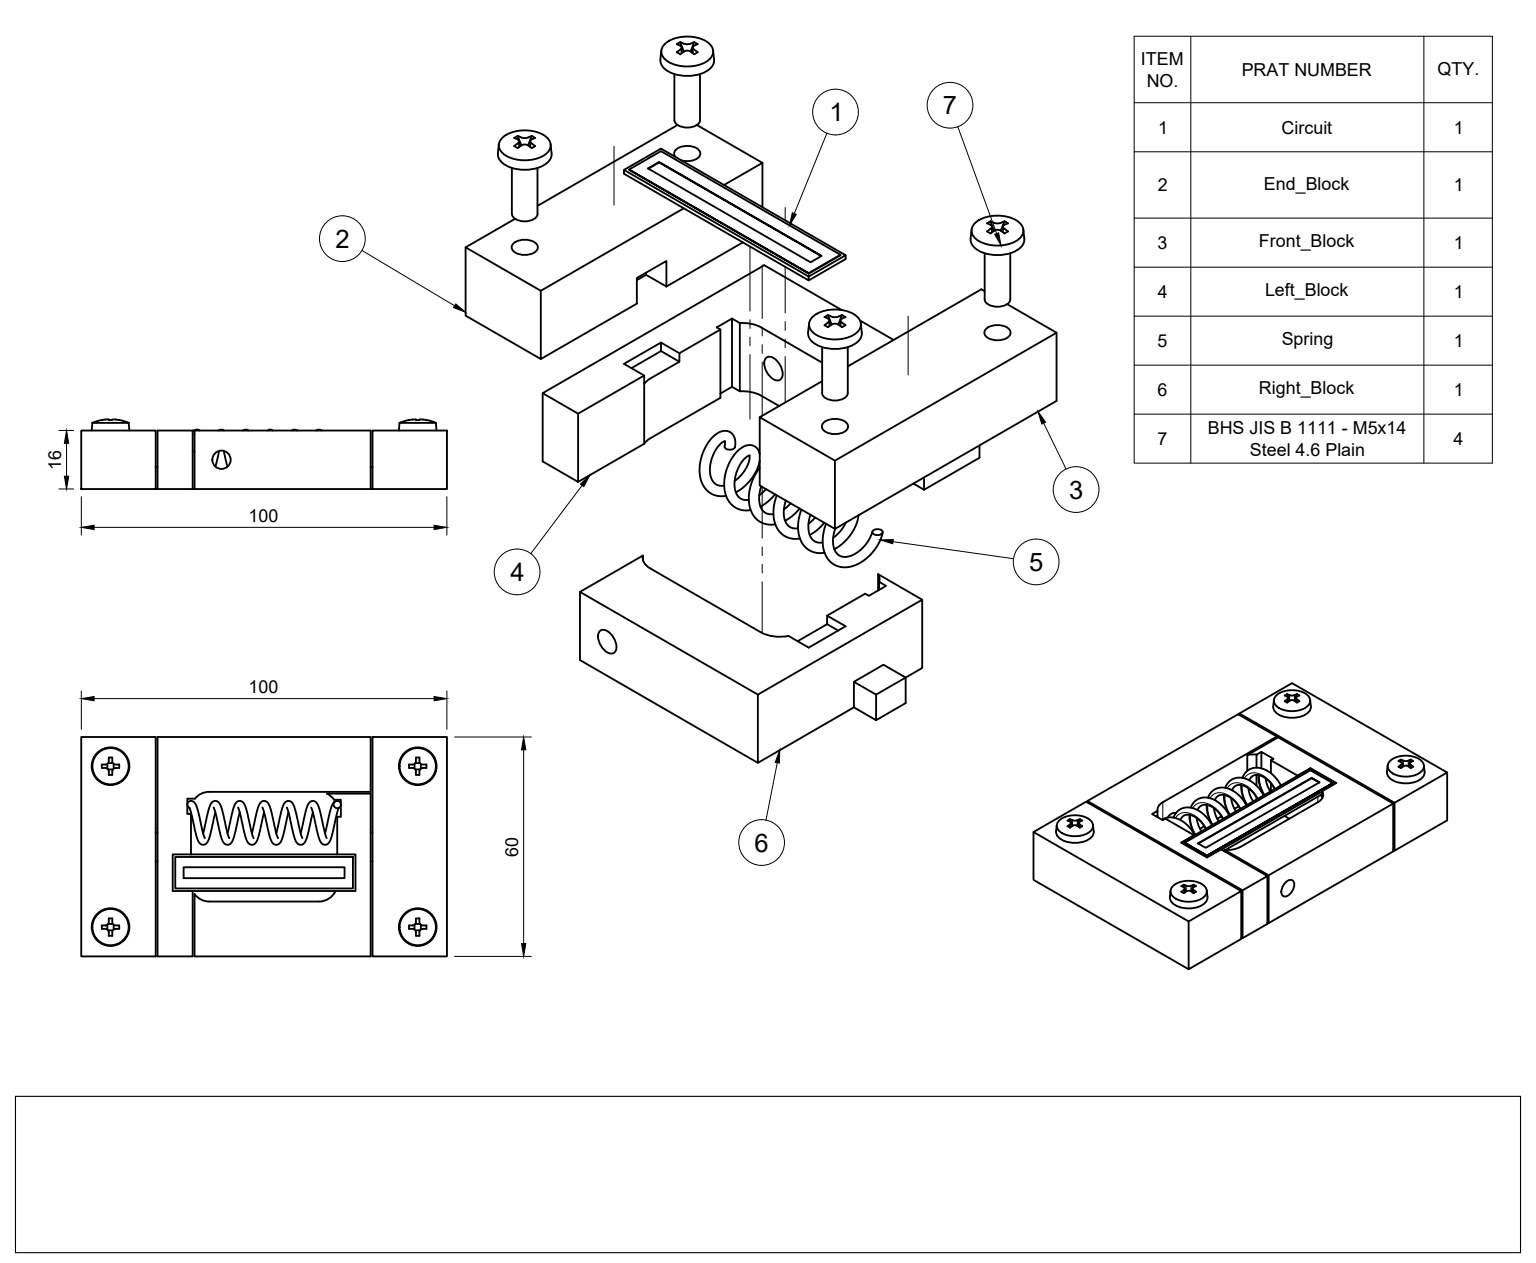
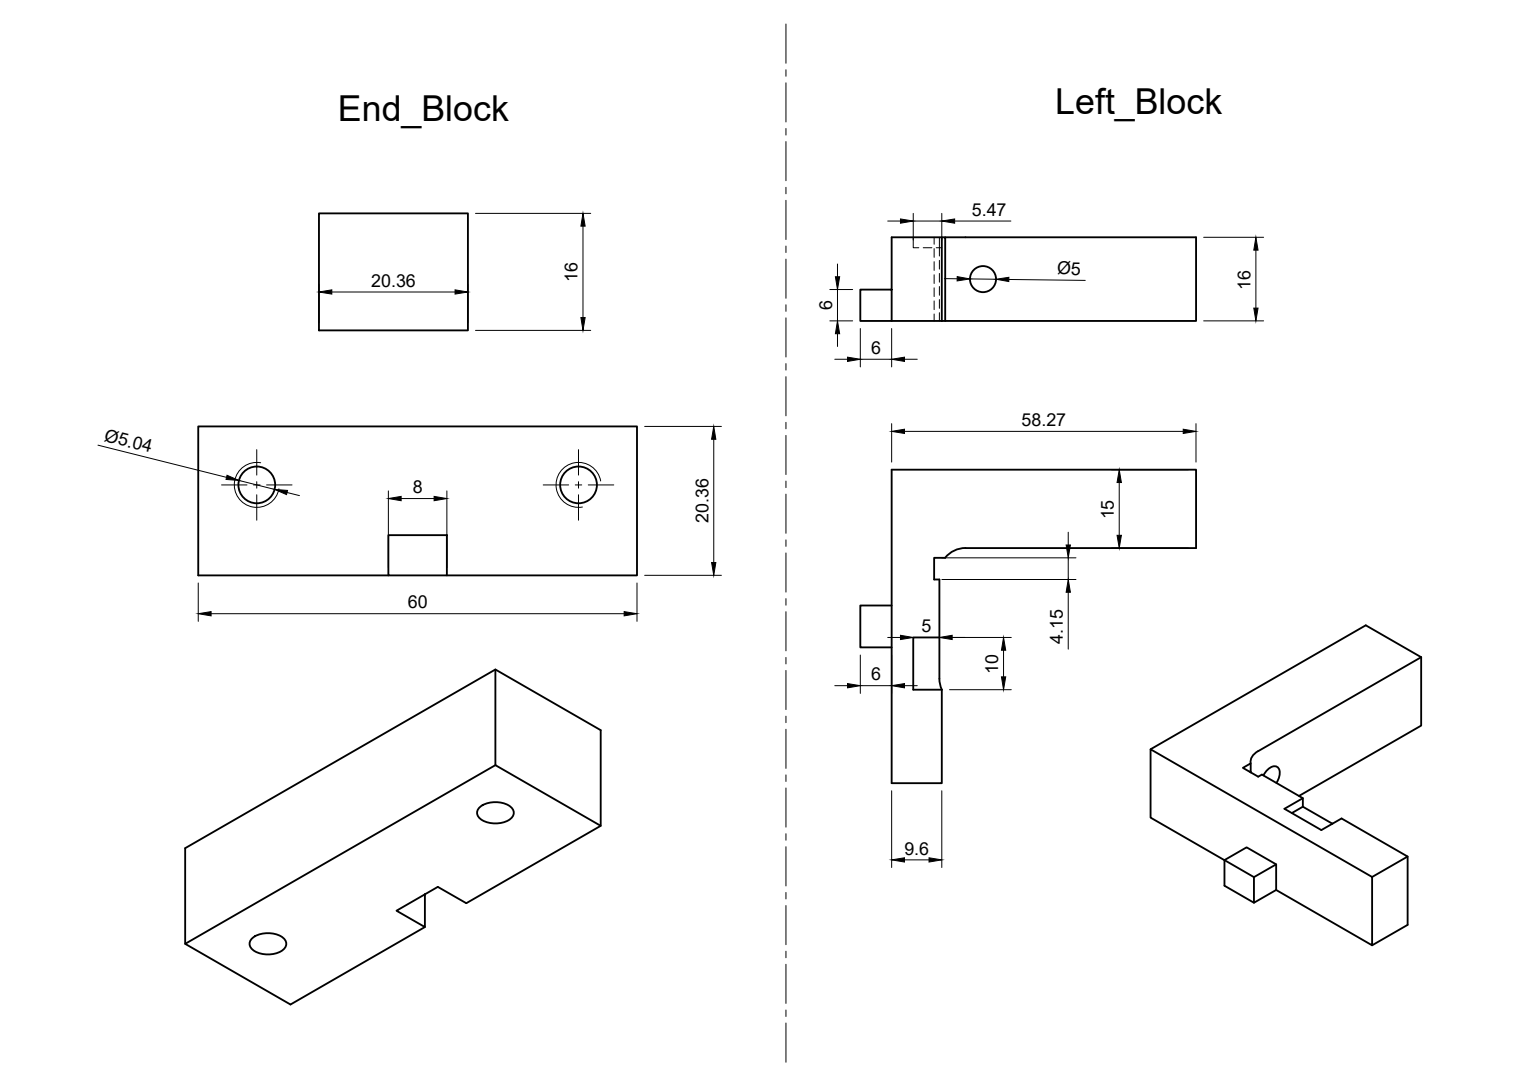
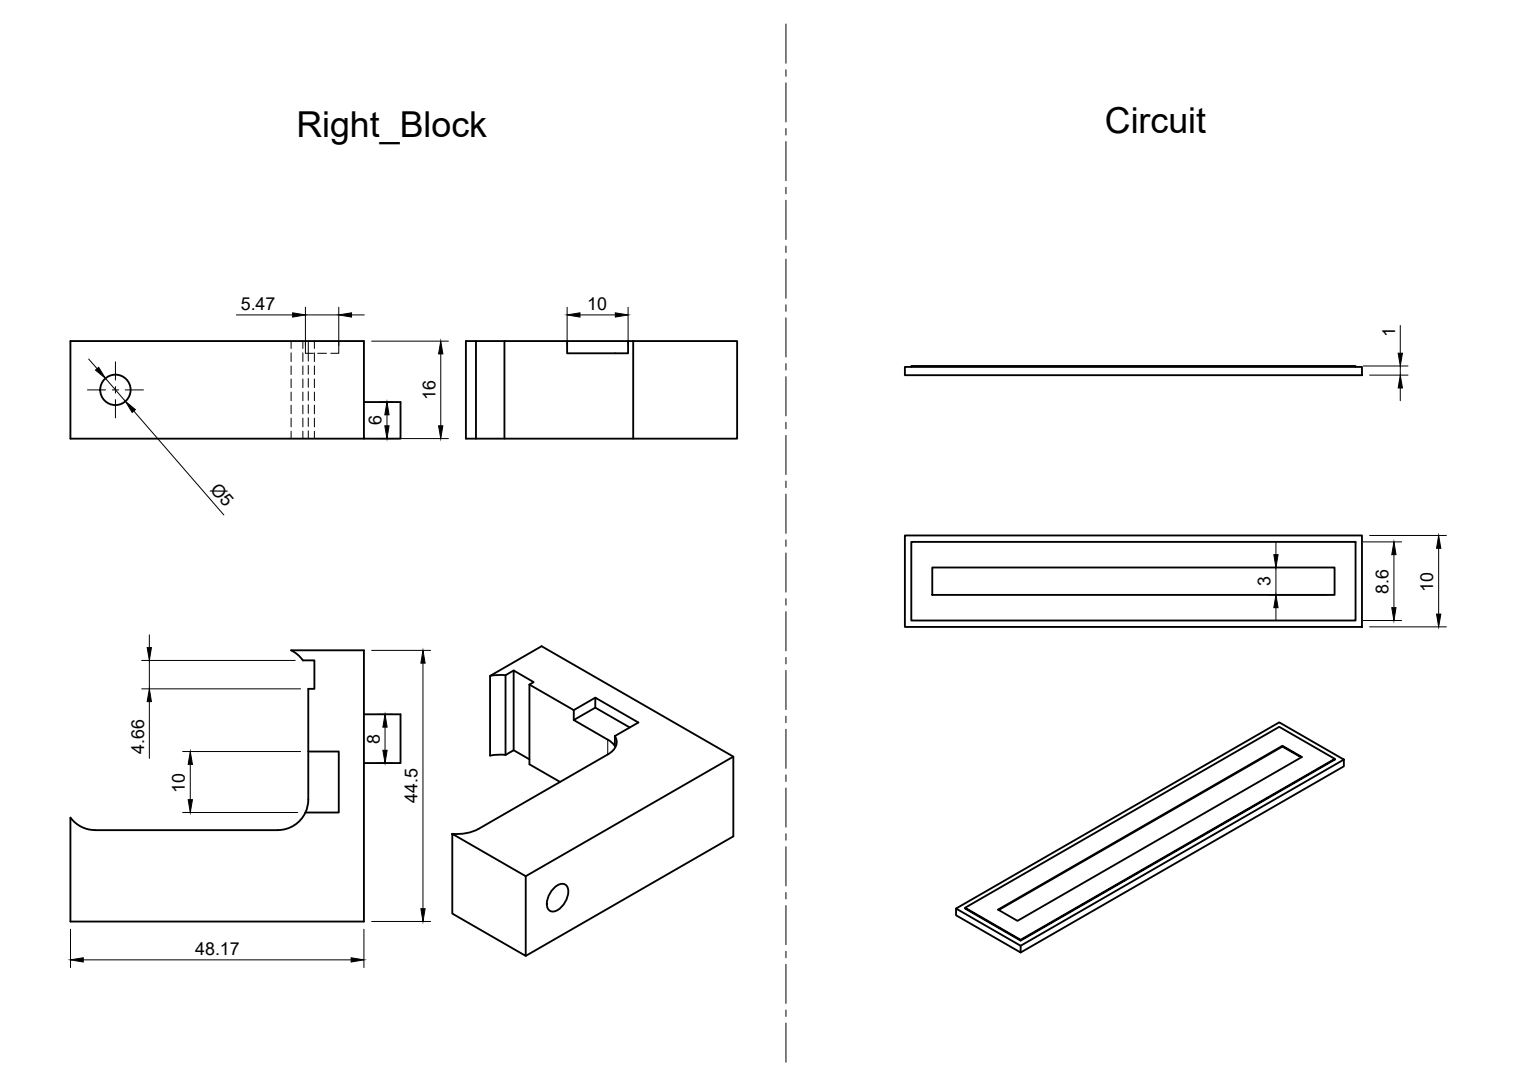
ISO-10303-21;
HEADER;
/* Generated by software containing ST-Developer
 * from STEP Tools, Inc. (www.steptools.com) 
 */

FILE_DESCRIPTION(
/* description */ (''),
/* implementation_level */ '2;1');

FILE_NAME(
/* name */ 'MAS-278',
/* time_stamp */ '2026-10-23T22:29:29+06:00',
/* author */ (''),
/* organization */ (''),
/* preprocessor_version */ 'ST-DEVELOPER v20.2',
/* originating_system */ 'Autodesk Translation Framework v15.15.0.0',
/* authorisation */ '');

FILE_SCHEMA (('AUTOMOTIVE_DESIGN { 1 0 10303 214 3 1 1 }'));
ENDSEC;

DATA;
#10=MECHANICAL_DESIGN_GEOMETRIC_PRESENTATION_REPRESENTATION('',(#72,#73,
#74,#75,#76,#77,#78,#79,#80,#81,#82,#83,#84),#7047);
#11=ITEM_DEFINED_TRANSFORMATION($,$,#3519,#3882);
#12=ITEM_DEFINED_TRANSFORMATION($,$,#3580,#3883);
#13=ITEM_DEFINED_TRANSFORMATION($,$,#3641,#3884);
#14=ITEM_DEFINED_TRANSFORMATION($,$,#3702,#3885);
#15=ITEM_DEFINED_TRANSFORMATION($,$,#3763,#3886);
#16=ITEM_DEFINED_TRANSFORMATION($,$,#3780,#3887);
#17=ITEM_DEFINED_TRANSFORMATION($,$,#3810,#3888);
#18=ITEM_DEFINED_TRANSFORMATION($,$,#3827,#3889);
#19=ITEM_DEFINED_TRANSFORMATION($,$,#3860,#3890);
#20=ITEM_DEFINED_TRANSFORMATION($,$,#3865,#3891);
#21=(
REPRESENTATION_RELATIONSHIP($,$,#7085,#7084)
REPRESENTATION_RELATIONSHIP_WITH_TRANSFORMATION(#11)
SHAPE_REPRESENTATION_RELATIONSHIP()
);
#22=(
REPRESENTATION_RELATIONSHIP($,$,#7086,#7084)
REPRESENTATION_RELATIONSHIP_WITH_TRANSFORMATION(#12)
SHAPE_REPRESENTATION_RELATIONSHIP()
);
#23=(
REPRESENTATION_RELATIONSHIP($,$,#7087,#7084)
REPRESENTATION_RELATIONSHIP_WITH_TRANSFORMATION(#13)
SHAPE_REPRESENTATION_RELATIONSHIP()
);
#24=(
REPRESENTATION_RELATIONSHIP($,$,#7088,#7084)
REPRESENTATION_RELATIONSHIP_WITH_TRANSFORMATION(#14)
SHAPE_REPRESENTATION_RELATIONSHIP()
);
#25=(
REPRESENTATION_RELATIONSHIP($,$,#7089,#7084)
REPRESENTATION_RELATIONSHIP_WITH_TRANSFORMATION(#15)
SHAPE_REPRESENTATION_RELATIONSHIP()
);
#26=(
REPRESENTATION_RELATIONSHIP($,$,#7090,#7084)
REPRESENTATION_RELATIONSHIP_WITH_TRANSFORMATION(#16)
SHAPE_REPRESENTATION_RELATIONSHIP()
);
#27=(
REPRESENTATION_RELATIONSHIP($,$,#7091,#7084)
REPRESENTATION_RELATIONSHIP_WITH_TRANSFORMATION(#17)
SHAPE_REPRESENTATION_RELATIONSHIP()
);
#28=(
REPRESENTATION_RELATIONSHIP($,$,#7092,#7084)
REPRESENTATION_RELATIONSHIP_WITH_TRANSFORMATION(#18)
SHAPE_REPRESENTATION_RELATIONSHIP()
);
#29=(
REPRESENTATION_RELATIONSHIP($,$,#7093,#7084)
REPRESENTATION_RELATIONSHIP_WITH_TRANSFORMATION(#19)
SHAPE_REPRESENTATION_RELATIONSHIP()
);
#30=(
REPRESENTATION_RELATIONSHIP($,$,#7094,#7084)
REPRESENTATION_RELATIONSHIP_WITH_TRANSFORMATION(#20)
SHAPE_REPRESENTATION_RELATIONSHIP()
);
#31=CONTEXT_DEPENDENT_SHAPE_REPRESENTATION(#21,#7074);
#32=CONTEXT_DEPENDENT_SHAPE_REPRESENTATION(#22,#7075);
#33=CONTEXT_DEPENDENT_SHAPE_REPRESENTATION(#23,#7076);
#34=CONTEXT_DEPENDENT_SHAPE_REPRESENTATION(#24,#7077);
#35=CONTEXT_DEPENDENT_SHAPE_REPRESENTATION(#25,#7078);
#36=CONTEXT_DEPENDENT_SHAPE_REPRESENTATION(#26,#7079);
#37=CONTEXT_DEPENDENT_SHAPE_REPRESENTATION(#27,#7080);
#38=CONTEXT_DEPENDENT_SHAPE_REPRESENTATION(#28,#7081);
#39=CONTEXT_DEPENDENT_SHAPE_REPRESENTATION(#29,#7082);
#40=CONTEXT_DEPENDENT_SHAPE_REPRESENTATION(#30,#7083);
#41=NEXT_ASSEMBLY_USAGE_OCCURRENCE('M5x14 Steel 4.6 Plain v1:1',
'M5x14 Steel 4.6 Plain v1:1','M5x14 Steel 4.6 Plain v1:1',#7096,#7097,
'M5x14 Steel 4.6 Plain v1:1');
#42=NEXT_ASSEMBLY_USAGE_OCCURRENCE('M5x14 Steel 4.6 Plain v1 (1):1',
'M5x14 Steel 4.6 Plain v1 (1):1','M5x14 Steel 4.6 Plain v1 (1):1',#7096,
#7098,'M5x14 Steel 4.6 Plain v1 (1):1');
#43=NEXT_ASSEMBLY_USAGE_OCCURRENCE('M5x14 Steel 4.6 Plain v1 (2):1',
'M5x14 Steel 4.6 Plain v1 (2):1','M5x14 Steel 4.6 Plain v1 (2):1',#7096,
#7099,'M5x14 Steel 4.6 Plain v1 (2):1');
#44=NEXT_ASSEMBLY_USAGE_OCCURRENCE('M5x14 Steel 4.6 Plain v1 (3):1',
'M5x14 Steel 4.6 Plain v1 (3):1','M5x14 Steel 4.6 Plain v1 (3):1',#7096,
#7100,'M5x14 Steel 4.6 Plain v1 (3):1');
#45=NEXT_ASSEMBLY_USAGE_OCCURRENCE('Front_Block:1','Front_Block:1',
'Front_Block:1',#7096,#7101,'Front_Block:1');
#46=NEXT_ASSEMBLY_USAGE_OCCURRENCE('Left_Block:1','Left_Block:1',
'Left_Block:1',#7096,#7102,'Left_Block:1');
#47=NEXT_ASSEMBLY_USAGE_OCCURRENCE('End_Block:1','End_Block:1',
'End_Block:1',#7096,#7103,'End_Block:1');
#48=NEXT_ASSEMBLY_USAGE_OCCURRENCE('Right_Block:1','Right_Block:1',
'Right_Block:1',#7096,#7104,'Right_Block:1');
#49=NEXT_ASSEMBLY_USAGE_OCCURRENCE('Spring:1','Spring:1','Spring:1',#7096,
#7105,'Spring:1');
#50=NEXT_ASSEMBLY_USAGE_OCCURRENCE('Circuit:1','Circuit:1','Circuit:1',
#7096,#7106,'Circuit:1');
#51=B_SPLINE_SURFACE_WITH_KNOTS('',3,3,((#6062,#6063,#6064,#6065,#6066,
#6067,#6068,#6069,#6070,#6071,#6072,#6073,#6074,#6075,#6076,#6077,#6078,
#6079,#6080,#6081,#6082,#6083,#6084,#6085,#6086,#6087,#6088,#6089,#6090,
#6091,#6092,#6093,#6094,#6095,#6096,#6097,#6098,#6099,#6100,#6101,#6102,
#6103,#6104,#6105,#6106,#6107,#6108,#6109,#6110,#6111,#6112,#6113,#6114,
#6115,#6116,#6117,#6118,#6119,#6120,#6121,#6122,#6123,#6124,#6125,#6126,
#6127,#6128,#6129,#6130,#6131,#6132,#6133,#6134,#6135,#6136,#6137,#6138,
#6139,#6140),(#6141,#6142,#6143,#6144,#6145,#6146,#6147,#6148,#6149,#6150,
#6151,#6152,#6153,#6154,#6155,#6156,#6157,#6158,#6159,#6160,#6161,#6162,
#6163,#6164,#6165,#6166,#6167,#6168,#6169,#6170,#6171,#6172,#6173,#6174,
#6175,#6176,#6177,#6178,#6179,#6180,#6181,#6182,#6183,#6184,#6185,#6186,
#6187,#6188,#6189,#6190,#6191,#6192,#6193,#6194,#6195,#6196,#6197,#6198,
#6199,#6200,#6201,#6202,#6203,#6204,#6205,#6206,#6207,#6208,#6209,#6210,
#6211,#6212,#6213,#6214,#6215,#6216,#6217,#6218,#6219),(#6220,#6221,#6222,
#6223,#6224,#6225,#6226,#6227,#6228,#6229,#6230,#6231,#6232,#6233,#6234,
#6235,#6236,#6237,#6238,#6239,#6240,#6241,#6242,#6243,#6244,#6245,#6246,
#6247,#6248,#6249,#6250,#6251,#6252,#6253,#6254,#6255,#6256,#6257,#6258,
#6259,#6260,#6261,#6262,#6263,#6264,#6265,#6266,#6267,#6268,#6269,#6270,
#6271,#6272,#6273,#6274,#6275,#6276,#6277,#6278,#6279,#6280,#6281,#6282,
#6283,#6284,#6285,#6286,#6287,#6288,#6289,#6290,#6291,#6292,#6293,#6294,
#6295,#6296,#6297,#6298),(#6299,#6300,#6301,#6302,#6303,#6304,#6305,#6306,
#6307,#6308,#6309,#6310,#6311,#6312,#6313,#6314,#6315,#6316,#6317,#6318,
#6319,#6320,#6321,#6322,#6323,#6324,#6325,#6326,#6327,#6328,#6329,#6330,
#6331,#6332,#6333,#6334,#6335,#6336,#6337,#6338,#6339,#6340,#6341,#6342,
#6343,#6344,#6345,#6346,#6347,#6348,#6349,#6350,#6351,#6352,#6353,#6354,
#6355,#6356,#6357,#6358,#6359,#6360,#6361,#6362,#6363,#6364,#6365,#6366,
#6367,#6368,#6369,#6370,#6371,#6372,#6373,#6374,#6375,#6376,#6377),(#6378,
#6379,#6380,#6381,#6382,#6383,#6384,#6385,#6386,#6387,#6388,#6389,#6390,
#6391,#6392,#6393,#6394,#6395,#6396,#6397,#6398,#6399,#6400,#6401,#6402,
#6403,#6404,#6405,#6406,#6407,#6408,#6409,#6410,#6411,#6412,#6413,#6414,
#6415,#6416,#6417,#6418,#6419,#6420,#6421,#6422,#6423,#6424,#6425,#6426,
#6427,#6428,#6429,#6430,#6431,#6432,#6433,#6434,#6435,#6436,#6437,#6438,
#6439,#6440,#6441,#6442,#6443,#6444,#6445,#6446,#6447,#6448,#6449,#6450,
#6451,#6452,#6453,#6454,#6455,#6456),(#6457,#6458,#6459,#6460,#6461,#6462,
#6463,#6464,#6465,#6466,#6467,#6468,#6469,#6470,#6471,#6472,#6473,#6474,
#6475,#6476,#6477,#6478,#6479,#6480,#6481,#6482,#6483,#6484,#6485,#6486,
#6487,#6488,#6489,#6490,#6491,#6492,#6493,#6494,#6495,#6496,#6497,#6498,
#6499,#6500,#6501,#6502,#6503,#6504,#6505,#6506,#6507,#6508,#6509,#6510,
#6511,#6512,#6513,#6514,#6515,#6516,#6517,#6518,#6519,#6520,#6521,#6522,
#6523,#6524,#6525,#6526,#6527,#6528,#6529,#6530,#6531,#6532,#6533,#6534,
#6535),(#6536,#6537,#6538,#6539,#6540,#6541,#6542,#6543,#6544,#6545,#6546,
#6547,#6548,#6549,#6550,#6551,#6552,#6553,#6554,#6555,#6556,#6557,#6558,
#6559,#6560,#6561,#6562,#6563,#6564,#6565,#6566,#6567,#6568,#6569,#6570,
#6571,#6572,#6573,#6574,#6575,#6576,#6577,#6578,#6579,#6580,#6581,#6582,
#6583,#6584,#6585,#6586,#6587,#6588,#6589,#6590,#6591,#6592,#6593,#6594,
#6595,#6596,#6597,#6598,#6599,#6600,#6601,#6602,#6603,#6604,#6605,#6606,
#6607,#6608,#6609,#6610,#6611,#6612,#6613,#6614),(#6615,#6616,#6617,#6618,
#6619,#6620,#6621,#6622,#6623,#6624,#6625,#6626,#6627,#6628,#6629,#6630,
#6631,#6632,#6633,#6634,#6635,#6636,#6637,#6638,#6639,#6640,#6641,#6642,
#6643,#6644,#6645,#6646,#6647,#6648,#6649,#6650,#6651,#6652,#6653,#6654,
#6655,#6656,#6657,#6658,#6659,#6660,#6661,#6662,#6663,#6664,#6665,#6666,
#6667,#6668,#6669,#6670,#6671,#6672,#6673,#6674,#6675,#6676,#6677,#6678,
#6679,#6680,#6681,#6682,#6683,#6684,#6685,#6686,#6687,#6688,#6689,#6690,
#6691,#6692,#6693),(#6694,#6695,#6696,#6697,#6698,#6699,#6700,#6701,#6702,
#6703,#6704,#6705,#6706,#6707,#6708,#6709,#6710,#6711,#6712,#6713,#6714,
#6715,#6716,#6717,#6718,#6719,#6720,#6721,#6722,#6723,#6724,#6725,#6726,
#6727,#6728,#6729,#6730,#6731,#6732,#6733,#6734,#6735,#6736,#6737,#6738,
#6739,#6740,#6741,#6742,#6743,#6744,#6745,#6746,#6747,#6748,#6749,#6750,
#6751,#6752,#6753,#6754,#6755,#6756,#6757,#6758,#6759,#6760,#6761,#6762,
#6763,#6764,#6765,#6766,#6767,#6768,#6769,#6770,#6771,#6772),(#6773,#6774,
#6775,#6776,#6777,#6778,#6779,#6780,#6781,#6782,#6783,#6784,#6785,#6786,
#6787,#6788,#6789,#6790,#6791,#6792,#6793,#6794,#6795,#6796,#6797,#6798,
#6799,#6800,#6801,#6802,#6803,#6804,#6805,#6806,#6807,#6808,#6809,#6810,
#6811,#6812,#6813,#6814,#6815,#6816,#6817,#6818,#6819,#6820,#6821,#6822,
#6823,#6824,#6825,#6826,#6827,#6828,#6829,#6830,#6831,#6832,#6833,#6834,
#6835,#6836,#6837,#6838,#6839,#6840,#6841,#6842,#6843,#6844,#6845,#6846,
#6847,#6848,#6849,#6850,#6851)),.UNSPECIFIED.,.T.,.F.,.F.,(4,1,1,1,1,1,
1,4),(4,1,1,1,1,1,1,1,1,1,1,1,1,1,1,1,1,1,1,1,1,1,1,1,1,1,1,1,1,1,1,1,1,
1,1,1,1,1,1,1,1,1,1,1,1,1,1,1,1,1,1,1,1,1,1,1,1,1,1,1,1,1,1,1,1,1,1,1,1,
1,1,1,1,1,1,1,4),(-3.14159265358979,-2.24399475256414,-1.34639685153848,
-0.448798950512828,0.448798950512828,1.34639685153848,2.24399475256414,
3.14159265358979),(0.,0.496040945303652,0.992081890607303,1.48812283591095,
1.98416378121461,2.48020472651826,2.97624567182191,3.47228661712556,3.96832756242921,
4.46436850773286,4.96040945303652,5.45645039834017,5.95249134364382,6.44853228894747,
6.94457323425112,7.44061417955477,7.93665512485842,8.43269607016208,8.92873701546573,
9.42477796076938,9.92081890607303,10.4168598513767,10.9129007966803,11.408941741984,
11.9049826872876,12.4010236325913,12.8970645778949,13.3931055231986,13.8891464685022,
14.3851874138059,14.8812283591095,15.3772693044132,15.8733102497168,16.3693511950205,
16.8653921403242,17.3614330856278,17.8574740309315,18.3535149762351,18.8495559215388,
19.3455968668424,19.8416378121461,20.3376787574497,20.8337197027534,21.329760648057,
21.8258015933607,22.3218425386643,22.817883483968,23.3139244292716,23.8099653745753,
24.3060063198789,24.8020472651826,25.2980882104862,25.7941291557899,26.2901701010935,
26.7862110463972,27.2822519917008,27.7782929370045,28.2743338823081,28.7703748276118,
29.2664157729154,29.7624567182191,30.2584976635227,30.7545386088264,31.25057955413,
31.7466204994337,32.2426614447374,32.738702390041,33.2347433353447,33.7307842806483,
34.226825225952,34.7228661712556,35.2189071165593,35.7149480618629,36.2109890071666,
36.7070299524702,37.2030708977739,37.6991118430775),.UNSPECIFIED.);
#52=SHAPE_REPRESENTATION_RELATIONSHIP('SRR','None',#7085,#62);
#53=SHAPE_REPRESENTATION_RELATIONSHIP('SRR','None',#7086,#63);
#54=SHAPE_REPRESENTATION_RELATIONSHIP('SRR','None',#7087,#64);
#55=SHAPE_REPRESENTATION_RELATIONSHIP('SRR','None',#7088,#65);
#56=SHAPE_REPRESENTATION_RELATIONSHIP('SRR','None',#7089,#66);
#57=SHAPE_REPRESENTATION_RELATIONSHIP('SRR','None',#7090,#67);
#58=SHAPE_REPRESENTATION_RELATIONSHIP('SRR','None',#7091,#68);
#59=SHAPE_REPRESENTATION_RELATIONSHIP('SRR','None',#7092,#69);
#60=SHAPE_REPRESENTATION_RELATIONSHIP('SRR','None',#7093,#70);
#61=SHAPE_REPRESENTATION_RELATIONSHIP('SRR','None',#7094,#71);
#62=ADVANCED_BREP_SHAPE_REPRESENTATION('',(#85),#7037);
#63=ADVANCED_BREP_SHAPE_REPRESENTATION('',(#86),#7038);
#64=ADVANCED_BREP_SHAPE_REPRESENTATION('',(#87),#7039);
#65=ADVANCED_BREP_SHAPE_REPRESENTATION('',(#88),#7040);
#66=ADVANCED_BREP_SHAPE_REPRESENTATION('',(#89),#7041);
#67=ADVANCED_BREP_SHAPE_REPRESENTATION('',(#90),#7042);
#68=ADVANCED_BREP_SHAPE_REPRESENTATION('',(#91),#7043);
#69=ADVANCED_BREP_SHAPE_REPRESENTATION('',(#92),#7044);
#70=ADVANCED_BREP_SHAPE_REPRESENTATION('',(#93),#7045);
#71=ADVANCED_BREP_SHAPE_REPRESENTATION('',(#94),#7046);
#72=STYLED_ITEM('',(#7212),#85);
#73=STYLED_ITEM('',(#7212),#86);
#74=STYLED_ITEM('',(#7212),#87);
#75=STYLED_ITEM('',(#7212),#88);
#76=STYLED_ITEM('',(#7177),#89);
#77=STYLED_ITEM('',(#7177),#90);
#78=STYLED_ITEM('',(#7177),#91);
#79=STYLED_ITEM('',(#7177),#92);
#80=STYLED_ITEM('',(#7198),#93);
#81=STYLED_ITEM('',(#7212),#3385);
#82=STYLED_ITEM('',(#7212),#3392);
#83=STYLED_ITEM('',(#7212),#3395);
#84=STYLED_ITEM('',(#7212),#94);
#85=MANIFOLD_SOLID_BREP('Body1',#3397);
#86=MANIFOLD_SOLID_BREP('Body1',#3398);
#87=MANIFOLD_SOLID_BREP('Body1',#3399);
#88=MANIFOLD_SOLID_BREP('Body1',#3400);
#89=MANIFOLD_SOLID_BREP('Front_Block',#3401);
#90=MANIFOLD_SOLID_BREP('Left_Block',#3402);
#91=MANIFOLD_SOLID_BREP('End_Block',#3403);
#92=MANIFOLD_SOLID_BREP('Right_Block',#3404);
#93=MANIFOLD_SOLID_BREP('Spring',#3405);
#94=MANIFOLD_SOLID_BREP('Circuit',#3406);
#95=SPHERICAL_SURFACE('',#3575,12.8319377609308);
#96=SPHERICAL_SURFACE('',#3636,12.8319377609308);
#97=SPHERICAL_SURFACE('',#3697,12.8319377609308);
#98=SPHERICAL_SURFACE('',#3758,12.8319377609308);
#99=CONICAL_SURFACE('',#3570,2.33923048454133,0.261799387799147);
#100=CONICAL_SURFACE('',#3579,5.05813690328693,0.0872664626099692);
#101=CONICAL_SURFACE('',#3631,2.33923048454133,0.261799387799147);
#102=CONICAL_SURFACE('',#3640,5.05813690328693,0.0872664626099692);
#103=CONICAL_SURFACE('',#3692,2.33923048454133,0.261799387799147);
#104=CONICAL_SURFACE('',#3701,5.05813690328693,0.0872664626099692);
#105=CONICAL_SURFACE('',#3753,2.33923048454133,0.261799387799147);
#106=CONICAL_SURFACE('',#3762,5.05813690328693,0.0872664626099692);
#107=FACE_BOUND('',#474,.T.);
#108=FACE_BOUND('',#500,.T.);
#109=FACE_BOUND('',#526,.T.);
#110=FACE_BOUND('',#552,.T.);
#111=FACE_BOUND('',#564,.T.);
#112=FACE_BOUND('',#565,.T.);
#113=FACE_BOUND('',#568,.T.);
#114=FACE_BOUND('',#569,.T.);
#115=FACE_BOUND('',#590,.T.);
#116=FACE_BOUND('',#593,.T.);
#117=FACE_BOUND('',#606,.T.);
#118=FACE_BOUND('',#607,.T.);
#119=FACE_BOUND('',#610,.T.);
#120=FACE_BOUND('',#611,.T.);
#121=FACE_BOUND('',#626,.T.);
#122=FACE_BOUND('',#639,.T.);
#123=FACE_BOUND('',#649,.T.);
#124=FACE_BOUND('',#660,.T.);
#125=TOROIDAL_SURFACE('',#3562,2.37846096908266,0.2);
#126=TOROIDAL_SURFACE('',#3623,2.37846096908266,0.2);
#127=TOROIDAL_SURFACE('',#3684,2.37846096908266,0.2);
#128=TOROIDAL_SURFACE('',#3745,2.37846096908266,0.2);
#129=PLANE('',#3524);
#130=PLANE('',#3526);
#131=PLANE('',#3529);
#132=PLANE('',#3534);
#133=PLANE('',#3536);
#134=PLANE('',#3539);
#135=PLANE('',#3545);
#136=PLANE('',#3550);
#137=PLANE('',#3552);
#138=PLANE('',#3554);
#139=PLANE('',#3557);
#140=PLANE('',#3559);
#141=PLANE('',#3561);
#142=PLANE('',#3566);
#143=PLANE('',#3574);
#144=PLANE('',#3585);
#145=PLANE('',#3587);
#146=PLANE('',#3590);
#147=PLANE('',#3595);
#148=PLANE('',#3597);
#149=PLANE('',#3600);
#150=PLANE('',#3606);
#151=PLANE('',#3611);
#152=PLANE('',#3613);
#153=PLANE('',#3615);
#154=PLANE('',#3618);
#155=PLANE('',#3620);
#156=PLANE('',#3622);
#157=PLANE('',#3627);
#158=PLANE('',#3635);
#159=PLANE('',#3646);
#160=PLANE('',#3648);
#161=PLANE('',#3651);
#162=PLANE('',#3656);
#163=PLANE('',#3658);
#164=PLANE('',#3661);
#165=PLANE('',#3667);
#166=PLANE('',#3672);
#167=PLANE('',#3674);
#168=PLANE('',#3676);
#169=PLANE('',#3679);
#170=PLANE('',#3681);
#171=PLANE('',#3683);
#172=PLANE('',#3688);
#173=PLANE('',#3696);
#174=PLANE('',#3707);
#175=PLANE('',#3709);
#176=PLANE('',#3712);
#177=PLANE('',#3717);
#178=PLANE('',#3719);
#179=PLANE('',#3722);
#180=PLANE('',#3728);
#181=PLANE('',#3733);
#182=PLANE('',#3735);
#183=PLANE('',#3737);
#184=PLANE('',#3740);
#185=PLANE('',#3742);
#186=PLANE('',#3744);
#187=PLANE('',#3749);
#188=PLANE('',#3757);
#189=PLANE('',#3764);
#190=PLANE('',#3765);
#191=PLANE('',#3766);
#192=PLANE('',#3767);
#193=PLANE('',#3768);
#194=PLANE('',#3771);
#195=PLANE('',#3772);
#196=PLANE('',#3775);
#197=PLANE('',#3776);
#198=PLANE('',#3779);
#199=PLANE('',#3781);
#200=PLANE('',#3782);
#201=PLANE('',#3783);
#202=PLANE('',#3784);
#203=PLANE('',#3785);
#204=PLANE('',#3789);
#205=PLANE('',#3790);
#206=PLANE('',#3791);
#207=PLANE('',#3792);
#208=PLANE('',#3793);
#209=PLANE('',#3794);
#210=PLANE('',#3795);
#211=PLANE('',#3796);
#212=PLANE('',#3798);
#213=PLANE('',#3802);
#214=PLANE('',#3803);
#215=PLANE('',#3805);
#216=PLANE('',#3806);
#217=PLANE('',#3808);
#218=PLANE('',#3809);
#219=PLANE('',#3811);
#220=PLANE('',#3812);
#221=PLANE('',#3813);
#222=PLANE('',#3814);
#223=PLANE('',#3815);
#224=PLANE('',#3816);
#225=PLANE('',#3819);
#226=PLANE('',#3820);
#227=PLANE('',#3823);
#228=PLANE('',#3826);
#229=PLANE('',#3828);
#230=PLANE('',#3829);
#231=PLANE('',#3830);
#232=PLANE('',#3831);
#233=PLANE('',#3832);
#234=PLANE('',#3833);
#235=PLANE('',#3834);
#236=PLANE('',#3838);
#237=PLANE('',#3841);
#238=PLANE('',#3843);
#239=PLANE('',#3847);
#240=PLANE('',#3848);
#241=PLANE('',#3849);
#242=PLANE('',#3850);
#243=PLANE('',#3853);
#244=PLANE('',#3854);
#245=PLANE('',#3855);
#246=PLANE('',#3858);
#247=PLANE('',#3859);
#248=PLANE('',#3863);
#249=PLANE('',#3864);
#250=PLANE('',#3866);
#251=PLANE('',#3867);
#252=PLANE('',#3868);
#253=PLANE('',#3869);
#254=PLANE('',#3870);
#255=PLANE('',#3871);
#256=PLANE('',#3872);
#257=PLANE('',#3873);
#258=PLANE('',#3874);
#259=PLANE('',#3875);
#260=PLANE('',#3876);
#261=PLANE('',#3877);
#262=PLANE('',#3878);
#263=PLANE('',#3879);
#264=PLANE('',#3880);
#265=PLANE('',#3881);
#266=FACE_OUTER_BOUND('',#455,.T.);
#267=FACE_OUTER_BOUND('',#456,.T.);
#268=FACE_OUTER_BOUND('',#457,.T.);
#269=FACE_OUTER_BOUND('',#458,.T.);
#270=FACE_OUTER_BOUND('',#459,.T.);
#271=FACE_OUTER_BOUND('',#460,.T.);
#272=FACE_OUTER_BOUND('',#461,.T.);
#273=FACE_OUTER_BOUND('',#462,.T.);
#274=FACE_OUTER_BOUND('',#463,.T.);
#275=FACE_OUTER_BOUND('',#464,.T.);
#276=FACE_OUTER_BOUND('',#465,.T.);
#277=FACE_OUTER_BOUND('',#466,.T.);
#278=FACE_OUTER_BOUND('',#467,.T.);
#279=FACE_OUTER_BOUND('',#468,.T.);
#280=FACE_OUTER_BOUND('',#469,.T.);
#281=FACE_OUTER_BOUND('',#470,.T.);
#282=FACE_OUTER_BOUND('',#471,.T.);
#283=FACE_OUTER_BOUND('',#472,.T.);
#284=FACE_OUTER_BOUND('',#473,.T.);
#285=FACE_OUTER_BOUND('',#475,.T.);
#286=FACE_OUTER_BOUND('',#476,.T.);
#287=FACE_OUTER_BOUND('',#477,.T.);
#288=FACE_OUTER_BOUND('',#478,.T.);
#289=FACE_OUTER_BOUND('',#479,.T.);
#290=FACE_OUTER_BOUND('',#480,.T.);
#291=FACE_OUTER_BOUND('',#481,.T.);
#292=FACE_OUTER_BOUND('',#482,.T.);
#293=FACE_OUTER_BOUND('',#483,.T.);
#294=FACE_OUTER_BOUND('',#484,.T.);
#295=FACE_OUTER_BOUND('',#485,.T.);
#296=FACE_OUTER_BOUND('',#486,.T.);
#297=FACE_OUTER_BOUND('',#487,.T.);
#298=FACE_OUTER_BOUND('',#488,.T.);
#299=FACE_OUTER_BOUND('',#489,.T.);
#300=FACE_OUTER_BOUND('',#490,.T.);
#301=FACE_OUTER_BOUND('',#491,.T.);
#302=FACE_OUTER_BOUND('',#492,.T.);
#303=FACE_OUTER_BOUND('',#493,.T.);
#304=FACE_OUTER_BOUND('',#494,.T.);
#305=FACE_OUTER_BOUND('',#495,.T.);
#306=FACE_OUTER_BOUND('',#496,.T.);
#307=FACE_OUTER_BOUND('',#497,.T.);
#308=FACE_OUTER_BOUND('',#498,.T.);
#309=FACE_OUTER_BOUND('',#499,.T.);
#310=FACE_OUTER_BOUND('',#501,.T.);
#311=FACE_OUTER_BOUND('',#502,.T.);
#312=FACE_OUTER_BOUND('',#503,.T.);
#313=FACE_OUTER_BOUND('',#504,.T.);
#314=FACE_OUTER_BOUND('',#505,.T.);
#315=FACE_OUTER_BOUND('',#506,.T.);
#316=FACE_OUTER_BOUND('',#507,.T.);
#317=FACE_OUTER_BOUND('',#508,.T.);
#318=FACE_OUTER_BOUND('',#509,.T.);
#319=FACE_OUTER_BOUND('',#510,.T.);
#320=FACE_OUTER_BOUND('',#511,.T.);
#321=FACE_OUTER_BOUND('',#512,.T.);
#322=FACE_OUTER_BOUND('',#513,.T.);
#323=FACE_OUTER_BOUND('',#514,.T.);
#324=FACE_OUTER_BOUND('',#515,.T.);
#325=FACE_OUTER_BOUND('',#516,.T.);
#326=FACE_OUTER_BOUND('',#517,.T.);
#327=FACE_OUTER_BOUND('',#518,.T.);
#328=FACE_OUTER_BOUND('',#519,.T.);
#329=FACE_OUTER_BOUND('',#520,.T.);
#330=FACE_OUTER_BOUND('',#521,.T.);
#331=FACE_OUTER_BOUND('',#522,.T.);
#332=FACE_OUTER_BOUND('',#523,.T.);
#333=FACE_OUTER_BOUND('',#524,.T.);
#334=FACE_OUTER_BOUND('',#525,.T.);
#335=FACE_OUTER_BOUND('',#527,.T.);
#336=FACE_OUTER_BOUND('',#528,.T.);
#337=FACE_OUTER_BOUND('',#529,.T.);
#338=FACE_OUTER_BOUND('',#530,.T.);
#339=FACE_OUTER_BOUND('',#531,.T.);
#340=FACE_OUTER_BOUND('',#532,.T.);
#341=FACE_OUTER_BOUND('',#533,.T.);
#342=FACE_OUTER_BOUND('',#534,.T.);
#343=FACE_OUTER_BOUND('',#535,.T.);
#344=FACE_OUTER_BOUND('',#536,.T.);
#345=FACE_OUTER_BOUND('',#537,.T.);
#346=FACE_OUTER_BOUND('',#538,.T.);
#347=FACE_OUTER_BOUND('',#539,.T.);
#348=FACE_OUTER_BOUND('',#540,.T.);
#349=FACE_OUTER_BOUND('',#541,.T.);
#350=FACE_OUTER_BOUND('',#542,.T.);
#351=FACE_OUTER_BOUND('',#543,.T.);
#352=FACE_OUTER_BOUND('',#544,.T.);
#353=FACE_OUTER_BOUND('',#545,.T.);
#354=FACE_OUTER_BOUND('',#546,.T.);
#355=FACE_OUTER_BOUND('',#547,.T.);
#356=FACE_OUTER_BOUND('',#548,.T.);
#357=FACE_OUTER_BOUND('',#549,.T.);
#358=FACE_OUTER_BOUND('',#550,.T.);
#359=FACE_OUTER_BOUND('',#551,.T.);
#360=FACE_OUTER_BOUND('',#553,.T.);
#361=FACE_OUTER_BOUND('',#554,.T.);
#362=FACE_OUTER_BOUND('',#555,.T.);
#363=FACE_OUTER_BOUND('',#556,.T.);
#364=FACE_OUTER_BOUND('',#557,.T.);
#365=FACE_OUTER_BOUND('',#558,.T.);
#366=FACE_OUTER_BOUND('',#559,.T.);
#367=FACE_OUTER_BOUND('',#560,.T.);
#368=FACE_OUTER_BOUND('',#561,.T.);
#369=FACE_OUTER_BOUND('',#562,.T.);
#370=FACE_OUTER_BOUND('',#563,.T.);
#371=FACE_OUTER_BOUND('',#566,.T.);
#372=FACE_OUTER_BOUND('',#567,.T.);
#373=FACE_OUTER_BOUND('',#570,.T.);
#374=FACE_OUTER_BOUND('',#571,.T.);
#375=FACE_OUTER_BOUND('',#572,.T.);
#376=FACE_OUTER_BOUND('',#573,.T.);
#377=FACE_OUTER_BOUND('',#574,.T.);
#378=FACE_OUTER_BOUND('',#575,.T.);
#379=FACE_OUTER_BOUND('',#576,.T.);
#380=FACE_OUTER_BOUND('',#577,.T.);
#381=FACE_OUTER_BOUND('',#578,.T.);
#382=FACE_OUTER_BOUND('',#579,.T.);
#383=FACE_OUTER_BOUND('',#580,.T.);
#384=FACE_OUTER_BOUND('',#581,.T.);
#385=FACE_OUTER_BOUND('',#582,.T.);
#386=FACE_OUTER_BOUND('',#583,.T.);
#387=FACE_OUTER_BOUND('',#584,.T.);
#388=FACE_OUTER_BOUND('',#585,.T.);
#389=FACE_OUTER_BOUND('',#586,.T.);
#390=FACE_OUTER_BOUND('',#587,.T.);
#391=FACE_OUTER_BOUND('',#588,.T.);
#392=FACE_OUTER_BOUND('',#589,.T.);
#393=FACE_OUTER_BOUND('',#591,.T.);
#394=FACE_OUTER_BOUND('',#592,.T.);
#395=FACE_OUTER_BOUND('',#594,.T.);
#396=FACE_OUTER_BOUND('',#595,.T.);
#397=FACE_OUTER_BOUND('',#596,.T.);
#398=FACE_OUTER_BOUND('',#597,.T.);
#399=FACE_OUTER_BOUND('',#598,.T.);
#400=FACE_OUTER_BOUND('',#599,.T.);
#401=FACE_OUTER_BOUND('',#600,.T.);
#402=FACE_OUTER_BOUND('',#601,.T.);
#403=FACE_OUTER_BOUND('',#602,.T.);
#404=FACE_OUTER_BOUND('',#603,.T.);
#405=FACE_OUTER_BOUND('',#604,.T.);
#406=FACE_OUTER_BOUND('',#605,.T.);
#407=FACE_OUTER_BOUND('',#608,.T.);
#408=FACE_OUTER_BOUND('',#609,.T.);
#409=FACE_OUTER_BOUND('',#612,.T.);
#410=FACE_OUTER_BOUND('',#613,.T.);
#411=FACE_OUTER_BOUND('',#614,.T.);
#412=FACE_OUTER_BOUND('',#615,.T.);
#413=FACE_OUTER_BOUND('',#616,.T.);
#414=FACE_OUTER_BOUND('',#617,.T.);
#415=FACE_OUTER_BOUND('',#618,.T.);
#416=FACE_OUTER_BOUND('',#619,.T.);
#417=FACE_OUTER_BOUND('',#620,.T.);
#418=FACE_OUTER_BOUND('',#621,.T.);
#419=FACE_OUTER_BOUND('',#622,.T.);
#420=FACE_OUTER_BOUND('',#623,.T.);
#421=FACE_OUTER_BOUND('',#624,.T.);
#422=FACE_OUTER_BOUND('',#625,.T.);
#423=FACE_OUTER_BOUND('',#627,.T.);
#424=FACE_OUTER_BOUND('',#628,.T.);
#425=FACE_OUTER_BOUND('',#629,.T.);
#426=FACE_OUTER_BOUND('',#630,.T.);
#427=FACE_OUTER_BOUND('',#631,.T.);
#428=FACE_OUTER_BOUND('',#632,.T.);
#429=FACE_OUTER_BOUND('',#633,.T.);
#430=FACE_OUTER_BOUND('',#634,.T.);
#431=FACE_OUTER_BOUND('',#635,.T.);
#432=FACE_OUTER_BOUND('',#636,.T.);
#433=FACE_OUTER_BOUND('',#637,.T.);
#434=FACE_OUTER_BOUND('',#638,.T.);
#435=FACE_OUTER_BOUND('',#640,.T.);
#436=FACE_OUTER_BOUND('',#641,.T.);
#437=FACE_OUTER_BOUND('',#642,.T.);
#438=FACE_OUTER_BOUND('',#643,.T.);
#439=FACE_OUTER_BOUND('',#644,.T.);
#440=FACE_OUTER_BOUND('',#645,.T.);
#441=FACE_OUTER_BOUND('',#646,.T.);
#442=FACE_OUTER_BOUND('',#647,.T.);
#443=FACE_OUTER_BOUND('',#648,.T.);
#444=FACE_OUTER_BOUND('',#650,.T.);
#445=FACE_OUTER_BOUND('',#651,.T.);
#446=FACE_OUTER_BOUND('',#652,.T.);
#447=FACE_OUTER_BOUND('',#653,.T.);
#448=FACE_OUTER_BOUND('',#654,.T.);
#449=FACE_OUTER_BOUND('',#655,.T.);
#450=FACE_OUTER_BOUND('',#656,.T.);
#451=FACE_OUTER_BOUND('',#657,.T.);
#452=FACE_OUTER_BOUND('',#658,.T.);
#453=FACE_OUTER_BOUND('',#659,.T.);
#454=FACE_OUTER_BOUND('',#661,.T.);
#455=EDGE_LOOP('',(#2221,#2222,#2223,#2224,#2225,#2226));
#456=EDGE_LOOP('',(#2227,#2228,#2229));
#457=EDGE_LOOP('',(#2230,#2231,#2232,#2233,#2234,#2235));
#458=EDGE_LOOP('',(#2236,#2237,#2238));
#459=EDGE_LOOP('',(#2239,#2240,#2241,#2242,#2243,#2244));
#460=EDGE_LOOP('',(#2245,#2246,#2247));
#461=EDGE_LOOP('',(#2248,#2249,#2250,#2251,#2252,#2253));
#462=EDGE_LOOP('',(#2254,#2255,#2256));
#463=EDGE_LOOP('',(#2257,#2258,#2259,#2260,#2261,#2262));
#464=EDGE_LOOP('',(#2263,#2264,#2265));
#465=EDGE_LOOP('',(#2266,#2267,#2268,#2269,#2270,#2271));
#466=EDGE_LOOP('',(#2272,#2273,#2274));
#467=EDGE_LOOP('',(#2275,#2276,#2277));
#468=EDGE_LOOP('',(#2278,#2279,#2280,#2281,#2282,#2283,#2284));
#469=EDGE_LOOP('',(#2285,#2286,#2287));
#470=EDGE_LOOP('',(#2288,#2289,#2290,#2291,#2292,#2293));
#471=EDGE_LOOP('',(#2294,#2295,#2296,#2297,#2298,#2299,#2300,#2301));
#472=EDGE_LOOP('',(#2302,#2303,#2304,#2305));
#473=EDGE_LOOP('',(#2306));
#474=EDGE_LOOP('',(#2307));
#475=EDGE_LOOP('',(#2308,#2309,#2310,#2311));
#476=EDGE_LOOP('',(#2312,#2313,#2314,#2315));
#477=EDGE_LOOP('',(#2316,#2317,#2318,#2319));
#478=EDGE_LOOP('',(#2320));
#479=EDGE_LOOP('',(#2321,#2322,#2323,#2324,#2325,#2326,#2327,#2328,#2329,
#2330,#2331,#2332,#2333,#2334,#2335,#2336,#2337,#2338,#2339,#2340,#2341));
#480=EDGE_LOOP('',(#2342,#2343,#2344,#2345,#2346));
#481=EDGE_LOOP('',(#2347,#2348,#2349,#2350,#2351,#2352));
#482=EDGE_LOOP('',(#2353,#2354,#2355));
#483=EDGE_LOOP('',(#2356,#2357,#2358,#2359,#2360,#2361));
#484=EDGE_LOOP('',(#2362,#2363,#2364));
#485=EDGE_LOOP('',(#2365,#2366,#2367,#2368,#2369,#2370));
#486=EDGE_LOOP('',(#2371,#2372,#2373));
#487=EDGE_LOOP('',(#2374,#2375,#2376,#2377,#2378,#2379));
#488=EDGE_LOOP('',(#2380,#2381,#2382));
#489=EDGE_LOOP('',(#2383,#2384,#2385,#2386,#2387,#2388));
#490=EDGE_LOOP('',(#2389,#2390,#2391));
#491=EDGE_LOOP('',(#2392,#2393,#2394,#2395,#2396,#2397));
#492=EDGE_LOOP('',(#2398,#2399,#2400));
#493=EDGE_LOOP('',(#2401,#2402,#2403));
#494=EDGE_LOOP('',(#2404,#2405,#2406,#2407,#2408,#2409,#2410));
#495=EDGE_LOOP('',(#2411,#2412,#2413));
#496=EDGE_LOOP('',(#2414,#2415,#2416,#2417,#2418,#2419));
#497=EDGE_LOOP('',(#2420,#2421,#2422,#2423,#2424,#2425,#2426,#2427));
#498=EDGE_LOOP('',(#2428,#2429,#2430,#2431));
#499=EDGE_LOOP('',(#2432));
#500=EDGE_LOOP('',(#2433));
#501=EDGE_LOOP('',(#2434,#2435,#2436,#2437));
#502=EDGE_LOOP('',(#2438,#2439,#2440,#2441));
#503=EDGE_LOOP('',(#2442,#2443,#2444,#2445));
#504=EDGE_LOOP('',(#2446));
#505=EDGE_LOOP('',(#2447,#2448,#2449,#2450,#2451,#2452,#2453,#2454,#2455,
#2456,#2457,#2458,#2459,#2460,#2461,#2462,#2463,#2464,#2465,#2466,#2467));
#506=EDGE_LOOP('',(#2468,#2469,#2470,#2471,#2472));
#507=EDGE_LOOP('',(#2473,#2474,#2475,#2476,#2477,#2478));
#508=EDGE_LOOP('',(#2479,#2480,#2481));
#509=EDGE_LOOP('',(#2482,#2483,#2484,#2485,#2486,#2487));
#510=EDGE_LOOP('',(#2488,#2489,#2490));
#511=EDGE_LOOP('',(#2491,#2492,#2493,#2494,#2495,#2496));
#512=EDGE_LOOP('',(#2497,#2498,#2499));
#513=EDGE_LOOP('',(#2500,#2501,#2502,#2503,#2504,#2505));
#514=EDGE_LOOP('',(#2506,#2507,#2508));
#515=EDGE_LOOP('',(#2509,#2510,#2511,#2512,#2513,#2514));
#516=EDGE_LOOP('',(#2515,#2516,#2517));
#517=EDGE_LOOP('',(#2518,#2519,#2520,#2521,#2522,#2523));
#518=EDGE_LOOP('',(#2524,#2525,#2526));
#519=EDGE_LOOP('',(#2527,#2528,#2529));
#520=EDGE_LOOP('',(#2530,#2531,#2532,#2533,#2534,#2535,#2536));
#521=EDGE_LOOP('',(#2537,#2538,#2539));
#522=EDGE_LOOP('',(#2540,#2541,#2542,#2543,#2544,#2545));
#523=EDGE_LOOP('',(#2546,#2547,#2548,#2549,#2550,#2551,#2552,#2553));
#524=EDGE_LOOP('',(#2554,#2555,#2556,#2557));
#525=EDGE_LOOP('',(#2558));
#526=EDGE_LOOP('',(#2559));
#527=EDGE_LOOP('',(#2560,#2561,#2562,#2563));
#528=EDGE_LOOP('',(#2564,#2565,#2566,#2567));
#529=EDGE_LOOP('',(#2568,#2569,#2570,#2571));
#530=EDGE_LOOP('',(#2572));
#531=EDGE_LOOP('',(#2573,#2574,#2575,#2576,#2577,#2578,#2579,#2580,#2581,
#2582,#2583,#2584,#2585,#2586,#2587,#2588,#2589,#2590,#2591,#2592,#2593));
#532=EDGE_LOOP('',(#2594,#2595,#2596,#2597,#2598));
#533=EDGE_LOOP('',(#2599,#2600,#2601,#2602,#2603,#2604));
#534=EDGE_LOOP('',(#2605,#2606,#2607));
#535=EDGE_LOOP('',(#2608,#2609,#2610,#2611,#2612,#2613));
#536=EDGE_LOOP('',(#2614,#2615,#2616));
#537=EDGE_LOOP('',(#2617,#2618,#2619,#2620,#2621,#2622));
#538=EDGE_LOOP('',(#2623,#2624,#2625));
#539=EDGE_LOOP('',(#2626,#2627,#2628,#2629,#2630,#2631));
#540=EDGE_LOOP('',(#2632,#2633,#2634));
#541=EDGE_LOOP('',(#2635,#2636,#2637,#2638,#2639,#2640));
#542=EDGE_LOOP('',(#2641,#2642,#2643));
#543=EDGE_LOOP('',(#2644,#2645,#2646,#2647,#2648,#2649));
#544=EDGE_LOOP('',(#2650,#2651,#2652));
#545=EDGE_LOOP('',(#2653,#2654,#2655));
#546=EDGE_LOOP('',(#2656,#2657,#2658,#2659,#2660,#2661,#2662));
#547=EDGE_LOOP('',(#2663,#2664,#2665));
#548=EDGE_LOOP('',(#2666,#2667,#2668,#2669,#2670,#2671));
#549=EDGE_LOOP('',(#2672,#2673,#2674,#2675,#2676,#2677,#2678,#2679));
#550=EDGE_LOOP('',(#2680,#2681,#2682,#2683));
#551=EDGE_LOOP('',(#2684));
#552=EDGE_LOOP('',(#2685));
#553=EDGE_LOOP('',(#2686,#2687,#2688,#2689));
#554=EDGE_LOOP('',(#2690,#2691,#2692,#2693));
#555=EDGE_LOOP('',(#2694,#2695,#2696,#2697));
#556=EDGE_LOOP('',(#2698));
#557=EDGE_LOOP('',(#2699,#2700,#2701,#2702,#2703,#2704,#2705,#2706,#2707,
#2708,#2709,#2710,#2711,#2712,#2713,#2714,#2715,#2716,#2717,#2718,#2719));
#558=EDGE_LOOP('',(#2720,#2721,#2722,#2723,#2724));
#559=EDGE_LOOP('',(#2725,#2726,#2727,#2728));
#560=EDGE_LOOP('',(#2729,#2730,#2731,#2732));
#561=EDGE_LOOP('',(#2733,#2734,#2735,#2736));
#562=EDGE_LOOP('',(#2737,#2738,#2739,#2740));
#563=EDGE_LOOP('',(#2741,#2742,#2743,#2744,#2745,#2746,#2747,#2748));
#564=EDGE_LOOP('',(#2749));
#565=EDGE_LOOP('',(#2750));
#566=EDGE_LOOP('',(#2751,#2752,#2753,#2754,#2755,#2756,#2757,#2758));
#567=EDGE_LOOP('',(#2759,#2760,#2761,#2762));
#568=EDGE_LOOP('',(#2763));
#569=EDGE_LOOP('',(#2764));
#570=EDGE_LOOP('',(#2765,#2766,#2767,#2768));
#571=EDGE_LOOP('',(#2769,#2770,#2771,#2772));
#572=EDGE_LOOP('',(#2773,#2774,#2775,#2776));
#573=EDGE_LOOP('',(#2777,#2778,#2779,#2780));
#574=EDGE_LOOP('',(#2781,#2782,#2783,#2784));
#575=EDGE_LOOP('',(#2785,#2786,#2787,#2788));
#576=EDGE_LOOP('',(#2789,#2790,#2791,#2792));
#577=EDGE_LOOP('',(#2793,#2794,#2795,#2796));
#578=EDGE_LOOP('',(#2797,#2798,#2799,#2800));
#579=EDGE_LOOP('',(#2801,#2802,#2803,#2804,#2805,#2806,#2807,#2808));
#580=EDGE_LOOP('',(#2809,#2810,#2811,#2812));
#581=EDGE_LOOP('',(#2813,#2814,#2815,#2816));
#582=EDGE_LOOP('',(#2817,#2818,#2819,#2820));
#583=EDGE_LOOP('',(#2821,#2822,#2823,#2824));
#584=EDGE_LOOP('',(#2825,#2826,#2827,#2828,#2829,#2830));
#585=EDGE_LOOP('',(#2831,#2832,#2833,#2834));
#586=EDGE_LOOP('',(#2835,#2836,#2837,#2838));
#587=EDGE_LOOP('',(#2839,#2840,#2841,#2842));
#588=EDGE_LOOP('',(#2843,#2844,#2845,#2846,#2847));
#589=EDGE_LOOP('',(#2848,#2849,#2850,#2851));
#590=EDGE_LOOP('',(#2852));
#591=EDGE_LOOP('',(#2853,#2854,#2855,#2856));
#592=EDGE_LOOP('',(#2857,#2858,#2859,#2860));
#593=EDGE_LOOP('',(#2861));
#594=EDGE_LOOP('',(#2862,#2863,#2864,#2865,#2866,#2867,#2868,#2869,#2870,
#2871,#2872,#2873,#2874,#2875,#2876,#2877));
#595=EDGE_LOOP('',(#2878,#2879,#2880,#2881));
#596=EDGE_LOOP('',(#2882,#2883,#2884,#2885,#2886,#2887,#2888,#2889,#2890,
#2891,#2892,#2893,#2894,#2895));
#597=EDGE_LOOP('',(#2896,#2897,#2898,#2899));
#598=EDGE_LOOP('',(#2900,#2901,#2902,#2903));
#599=EDGE_LOOP('',(#2904,#2905,#2906,#2907,#2908));
#600=EDGE_LOOP('',(#2909,#2910,#2911,#2912));
#601=EDGE_LOOP('',(#2913,#2914,#2915,#2916));
#602=EDGE_LOOP('',(#2917,#2918,#2919,#2920));
#603=EDGE_LOOP('',(#2921,#2922,#2923,#2924));
#604=EDGE_LOOP('',(#2925,#2926,#2927,#2928,#2929,#2930,#2931,#2932));
#605=EDGE_LOOP('',(#2933,#2934,#2935,#2936));
#606=EDGE_LOOP('',(#2937));
#607=EDGE_LOOP('',(#2938));
#608=EDGE_LOOP('',(#2939,#2940,#2941,#2942));
#609=EDGE_LOOP('',(#2943,#2944,#2945,#2946,#2947,#2948,#2949,#2950));
#610=EDGE_LOOP('',(#2951));
#611=EDGE_LOOP('',(#2952));
#612=EDGE_LOOP('',(#2953,#2954,#2955,#2956));
#613=EDGE_LOOP('',(#2957,#2958,#2959,#2960));
#614=EDGE_LOOP('',(#2961,#2962,#2963,#2964));
#615=EDGE_LOOP('',(#2965,#2966,#2967,#2968));
#616=EDGE_LOOP('',(#2969,#2970,#2971,#2972));
#617=EDGE_LOOP('',(#2973,#2974,#2975,#2976));
#618=EDGE_LOOP('',(#2977,#2978,#2979,#2980));
#619=EDGE_LOOP('',(#2981,#2982,#2983,#2984));
#620=EDGE_LOOP('',(#2985,#2986,#2987,#2988,#2989,#2990,#2991,#2992));
#621=EDGE_LOOP('',(#2993,#2994,#2995,#2996));
#622=EDGE_LOOP('',(#2997,#2998,#2999,#3000));
#623=EDGE_LOOP('',(#3001,#3002,#3003,#3004));
#624=EDGE_LOOP('',(#3005,#3006,#3007,#3008,#3009,#3010,#3011,#3012,#3013,
#3014,#3015,#3016,#3017,#3018,#3019,#3020));
#625=EDGE_LOOP('',(#3021,#3022,#3023,#3024));
#626=EDGE_LOOP('',(#3025));
#627=EDGE_LOOP('',(#3026,#3027,#3028,#3029,#3030,#3031));
#628=EDGE_LOOP('',(#3032,#3033,#3034,#3035,#3036,#3037));
#629=EDGE_LOOP('',(#3038,#3039,#3040,#3041));
#630=EDGE_LOOP('',(#3042,#3043,#3044,#3045));
#631=EDGE_LOOP('',(#3046,#3047,#3048,#3049,#3050));
#632=EDGE_LOOP('',(#3051,#3052,#3053,#3054));
#633=EDGE_LOOP('',(#3055,#3056,#3057,#3058));
#634=EDGE_LOOP('',(#3059,#3060,#3061,#3062));
#635=EDGE_LOOP('',(#3063,#3064,#3065,#3066));
#636=EDGE_LOOP('',(#3067,#3068,#3069,#3070));
#637=EDGE_LOOP('',(#3071,#3072,#3073,#3074));
#638=EDGE_LOOP('',(#3075,#3076,#3077,#3078));
#639=EDGE_LOOP('',(#3079));
#640=EDGE_LOOP('',(#3080,#3081,#3082,#3083,#3084,#3085,#3086,#3087,#3088,
#3089,#3090,#3091,#3092,#3093,#3094));
#641=EDGE_LOOP('',(#3095,#3096,#3097,#3098));
#642=EDGE_LOOP('',(#3099));
#643=EDGE_LOOP('',(#3100));
#644=EDGE_LOOP('',(#3101,#3102,#3103,#3104));
#645=EDGE_LOOP('',(#3105,#3106,#3107,#3108));
#646=EDGE_LOOP('',(#3109,#3110,#3111,#3112));
#647=EDGE_LOOP('',(#3113,#3114,#3115,#3116));
#648=EDGE_LOOP('',(#3117,#3118,#3119,#3120));
#649=EDGE_LOOP('',(#3121,#3122,#3123,#3124));
#650=EDGE_LOOP('',(#3125,#3126,#3127,#3128));
#651=EDGE_LOOP('',(#3129,#3130,#3131,#3132));
#652=EDGE_LOOP('',(#3133,#3134,#3135,#3136));
#653=EDGE_LOOP('',(#3137,#3138,#3139,#3140));
#654=EDGE_LOOP('',(#3141,#3142,#3143,#3144));
#655=EDGE_LOOP('',(#3145,#3146,#3147,#3148));
#656=EDGE_LOOP('',(#3149,#3150,#3151,#3152));
#657=EDGE_LOOP('',(#3153,#3154,#3155,#3156));
#658=EDGE_LOOP('',(#3157,#3158,#3159,#3160));
#659=EDGE_LOOP('',(#3161,#3162,#3163,#3164));
#660=EDGE_LOOP('',(#3165,#3166,#3167,#3168));
#661=EDGE_LOOP('',(#3169,#3170,#3171,#3172));
#662=CIRCLE('',#3522,0.946);
#663=CIRCLE('',#3525,12.8232171353527);
#664=CIRCLE('',#3527,12.1073709048319);
#665=CIRCLE('',#3530,12.8232171353527);
#666=CIRCLE('',#3532,0.946);
#667=CIRCLE('',#3535,12.8232171353527);
#668=CIRCLE('',#3537,12.1073709048319);
#669=CIRCLE('',#3540,12.8232171353527);
#670=CIRCLE('',#3543,0.946);
#671=CIRCLE('',#3546,12.8232171353527);
#672=CIRCLE('',#3548,0.946);
#673=CIRCLE('',#3551,12.8232171353527);
#674=CIRCLE('',#3553,12.8232171353527);
#675=CIRCLE('',#3555,12.1073709048319);
#676=CIRCLE('',#3556,12.1073709048319);
#677=CIRCLE('',#3558,12.8232171353527);
#678=CIRCLE('',#3560,12.1073709048319);
#679=CIRCLE('',#3563,2.37846096908266);
#680=CIRCLE('',#3564,0.2);
#681=CIRCLE('',#3565,2.17846096908266);
#682=CIRCLE('',#3567,5.15);
#683=CIRCLE('',#3569,2.17846096908266);
#684=CIRCLE('',#3571,2.4505);
#685=CIRCLE('',#3573,2.4505);
#686=CIRCLE('',#3576,12.8319377609308);
#687=CIRCLE('',#3577,4.96627380657387);
#688=CIRCLE('',#3578,4.96627380657387);
#689=CIRCLE('',#3583,0.946);
#690=CIRCLE('',#3586,12.8232171353527);
#691=CIRCLE('',#3588,12.1073709048319);
#692=CIRCLE('',#3591,12.8232171353527);
#693=CIRCLE('',#3593,0.946);
#694=CIRCLE('',#3596,12.8232171353527);
#695=CIRCLE('',#3598,12.1073709048319);
#696=CIRCLE('',#3601,12.8232171353527);
#697=CIRCLE('',#3604,0.946);
#698=CIRCLE('',#3607,12.8232171353527);
#699=CIRCLE('',#3609,0.946);
#700=CIRCLE('',#3612,12.8232171353527);
#701=CIRCLE('',#3614,12.8232171353527);
#702=CIRCLE('',#3616,12.1073709048319);
#703=CIRCLE('',#3617,12.1073709048319);
#704=CIRCLE('',#3619,12.8232171353527);
#705=CIRCLE('',#3621,12.1073709048319);
#706=CIRCLE('',#3624,2.37846096908266);
#707=CIRCLE('',#3625,0.2);
#708=CIRCLE('',#3626,2.17846096908266);
#709=CIRCLE('',#3628,5.15);
#710=CIRCLE('',#3630,2.17846096908266);
#711=CIRCLE('',#3632,2.4505);
#712=CIRCLE('',#3634,2.4505);
#713=CIRCLE('',#3637,12.8319377609308);
#714=CIRCLE('',#3638,4.96627380657387);
#715=CIRCLE('',#3639,4.96627380657387);
#716=CIRCLE('',#3644,0.946);
#717=CIRCLE('',#3647,12.8232171353527);
#718=CIRCLE('',#3649,12.1073709048319);
#719=CIRCLE('',#3652,12.8232171353527);
#720=CIRCLE('',#3654,0.946);
#721=CIRCLE('',#3657,12.8232171353527);
#722=CIRCLE('',#3659,12.1073709048319);
#723=CIRCLE('',#3662,12.8232171353527);
#724=CIRCLE('',#3665,0.946);
#725=CIRCLE('',#3668,12.8232171353527);
#726=CIRCLE('',#3670,0.946);
#727=CIRCLE('',#3673,12.8232171353527);
#728=CIRCLE('',#3675,12.8232171353527);
#729=CIRCLE('',#3677,12.1073709048319);
#730=CIRCLE('',#3678,12.1073709048319);
#731=CIRCLE('',#3680,12.8232171353527);
#732=CIRCLE('',#3682,12.1073709048319);
#733=CIRCLE('',#3685,2.37846096908266);
#734=CIRCLE('',#3686,0.2);
#735=CIRCLE('',#3687,2.17846096908266);
#736=CIRCLE('',#3689,5.15);
#737=CIRCLE('',#3691,2.17846096908266);
#738=CIRCLE('',#3693,2.4505);
#739=CIRCLE('',#3695,2.4505);
#740=CIRCLE('',#3698,12.8319377609308);
#741=CIRCLE('',#3699,4.96627380657387);
#742=CIRCLE('',#3700,4.96627380657387);
#743=CIRCLE('',#3705,0.946);
#744=CIRCLE('',#3708,12.8232171353527);
#745=CIRCLE('',#3710,12.1073709048319);
#746=CIRCLE('',#3713,12.8232171353527);
#747=CIRCLE('',#3715,0.946);
#748=CIRCLE('',#3718,12.8232171353527);
#749=CIRCLE('',#3720,12.1073709048319);
#750=CIRCLE('',#3723,12.8232171353527);
#751=CIRCLE('',#3726,0.946);
#752=CIRCLE('',#3729,12.8232171353527);
#753=CIRCLE('',#3731,0.946);
#754=CIRCLE('',#3734,12.8232171353527);
#755=CIRCLE('',#3736,12.8232171353527);
#756=CIRCLE('',#3738,12.1073709048319);
#757=CIRCLE('',#3739,12.1073709048319);
#758=CIRCLE('',#3741,12.8232171353527);
#759=CIRCLE('',#3743,12.1073709048319);
#760=CIRCLE('',#3746,2.37846096908266);
#761=CIRCLE('',#3747,0.2);
#762=CIRCLE('',#3748,2.17846096908266);
#763=CIRCLE('',#3750,5.15);
#764=CIRCLE('',#3752,2.17846096908266);
#765=CIRCLE('',#3754,2.4505);
#766=CIRCLE('',#3756,2.4505);
#767=CIRCLE('',#3759,12.8319377609308);
#768=CIRCLE('',#3760,4.96627380657387);
#769=CIRCLE('',#3761,4.96627380657387);
#770=CIRCLE('',#3769,2.5175);
#771=CIRCLE('',#3770,2.5175);
#772=CIRCLE('',#3773,2.5175);
#773=CIRCLE('',#3774,2.5175);
#774=CIRCLE('',#3787,2.5);
#775=CIRCLE('',#3788,2.5);
#776=CIRCLE('',#3797,4.99999999999999);
#777=CIRCLE('',#3800,4.99999999999999);
#778=CIRCLE('',#3801,4.99999999999999);
#779=CIRCLE('',#3804,4.99999999999999);
#780=CIRCLE('',#3817,2.5175);
#781=CIRCLE('',#3818,2.5175);
#782=CIRCLE('',#3821,2.5175);
#783=CIRCLE('',#3822,2.5175);
#784=CIRCLE('',#3836,4.99999999999999);
#785=CIRCLE('',#3837,4.99999999999999);
#786=CIRCLE('',#3839,4.99999999999999);
#787=CIRCLE('',#3840,4.99999999999999);
#788=CIRCLE('',#3842,2.5);
#789=CIRCLE('',#3845,4.99999999999999);
#790=CIRCLE('',#3846,4.99999999999999);
#791=CIRCLE('',#3852,4.99999999999999);
#792=CIRCLE('',#3857,2.5);
#793=CIRCLE('',#3861,1.);
#794=CIRCLE('',#3862,1.);
#795=ELLIPSE('',#3521,1.892,0.946);
#796=ELLIPSE('',#3523,1.892,0.946);
#797=ELLIPSE('',#3528,1.892,0.946);
#798=ELLIPSE('',#3533,1.892,0.946);
#799=ELLIPSE('',#3538,1.892,0.946);
#800=ELLIPSE('',#3542,1.892,0.946);
#801=ELLIPSE('',#3544,1.892,0.946);
#802=ELLIPSE('',#3549,1.892,0.946);
#803=ELLIPSE('',#3582,1.892,0.946);
#804=ELLIPSE('',#3584,1.892,0.946);
#805=ELLIPSE('',#3589,1.892,0.946);
#806=ELLIPSE('',#3594,1.892,0.946);
#807=ELLIPSE('',#3599,1.892,0.946);
#808=ELLIPSE('',#3603,1.892,0.946);
#809=ELLIPSE('',#3605,1.892,0.946);
#810=ELLIPSE('',#3610,1.892,0.946);
#811=ELLIPSE('',#3643,1.892,0.946);
#812=ELLIPSE('',#3645,1.892,0.946);
#813=ELLIPSE('',#3650,1.892,0.946);
#814=ELLIPSE('',#3655,1.892,0.946);
#815=ELLIPSE('',#3660,1.892,0.946);
#816=ELLIPSE('',#3664,1.892,0.946);
#817=ELLIPSE('',#3666,1.892,0.946);
#818=ELLIPSE('',#3671,1.892,0.946);
#819=ELLIPSE('',#3704,1.892,0.946);
#820=ELLIPSE('',#3706,1.892,0.946);
#821=ELLIPSE('',#3711,1.892,0.946);
#822=ELLIPSE('',#3716,1.892,0.946);
#823=ELLIPSE('',#3721,1.892,0.946);
#824=ELLIPSE('',#3725,1.892,0.946);
#825=ELLIPSE('',#3727,1.892,0.946);
#826=ELLIPSE('',#3732,1.892,0.946);
#827=LINE('',#4955,#1121);
#828=LINE('',#4962,#1122);
#829=LINE('',#4966,#1123);
#830=LINE('',#4971,#1124);
#831=LINE('',#4974,#1125);
#832=LINE('',#4978,#1126);
#833=LINE('',#5000,#1127);
#834=LINE('',#5004,#1128);
#835=LINE('',#5009,#1129);
#836=LINE('',#5012,#1130);
#837=LINE('',#5016,#1131);
#838=LINE('',#5036,#1132);
#839=LINE('',#5043,#1133);
#840=LINE('',#5047,#1134);
#841=LINE('',#5069,#1135);
#842=LINE('',#5073,#1136);
#843=LINE('',#5077,#1137);
#844=LINE('',#5081,#1138);
#845=LINE('',#5086,#1139);
#846=LINE('',#5089,#1140);
#847=LINE('',#5103,#1141);
#848=LINE('',#5107,#1142);
#849=LINE('',#5111,#1143);
#850=LINE('',#5120,#1144);
#851=LINE('',#5141,#1145);
#852=LINE('',#5148,#1146);
#853=LINE('',#5152,#1147);
#854=LINE('',#5157,#1148);
#855=LINE('',#5160,#1149);
#856=LINE('',#5164,#1150);
#857=LINE('',#5186,#1151);
#858=LINE('',#5190,#1152);
#859=LINE('',#5195,#1153);
#860=LINE('',#5198,#1154);
#861=LINE('',#5202,#1155);
#862=LINE('',#5222,#1156);
#863=LINE('',#5229,#1157);
#864=LINE('',#5233,#1158);
#865=LINE('',#5255,#1159);
#866=LINE('',#5259,#1160);
#867=LINE('',#5263,#1161);
#868=LINE('',#5267,#1162);
#869=LINE('',#5272,#1163);
#870=LINE('',#5275,#1164);
#871=LINE('',#5289,#1165);
#872=LINE('',#5293,#1166);
#873=LINE('',#5297,#1167);
#874=LINE('',#5306,#1168);
#875=LINE('',#5327,#1169);
#876=LINE('',#5334,#1170);
#877=LINE('',#5338,#1171);
#878=LINE('',#5343,#1172);
#879=LINE('',#5346,#1173);
#880=LINE('',#5350,#1174);
#881=LINE('',#5372,#1175);
#882=LINE('',#5376,#1176);
#883=LINE('',#5381,#1177);
#884=LINE('',#5384,#1178);
#885=LINE('',#5388,#1179);
#886=LINE('',#5408,#1180);
#887=LINE('',#5415,#1181);
#888=LINE('',#5419,#1182);
#889=LINE('',#5441,#1183);
#890=LINE('',#5445,#1184);
#891=LINE('',#5449,#1185);
#892=LINE('',#5453,#1186);
#893=LINE('',#5458,#1187);
#894=LINE('',#5461,#1188);
#895=LINE('',#5475,#1189);
#896=LINE('',#5479,#1190);
#897=LINE('',#5483,#1191);
#898=LINE('',#5492,#1192);
#899=LINE('',#5513,#1193);
#900=LINE('',#5520,#1194);
#901=LINE('',#5524,#1195);
#902=LINE('',#5529,#1196);
#903=LINE('',#5532,#1197);
#904=LINE('',#5536,#1198);
#905=LINE('',#5558,#1199);
#906=LINE('',#5562,#1200);
#907=LINE('',#5567,#1201);
#908=LINE('',#5570,#1202);
#909=LINE('',#5574,#1203);
#910=LINE('',#5594,#1204);
#911=LINE('',#5601,#1205);
#912=LINE('',#5605,#1206);
#913=LINE('',#5627,#1207);
#914=LINE('',#5631,#1208);
#915=LINE('',#5635,#1209);
#916=LINE('',#5639,#1210);
#917=LINE('',#5644,#1211);
#918=LINE('',#5647,#1212);
#919=LINE('',#5661,#1213);
#920=LINE('',#5665,#1214);
#921=LINE('',#5669,#1215);
#922=LINE('',#5678,#1216);
#923=LINE('',#5683,#1217);
#924=LINE('',#5685,#1218);
#925=LINE('',#5687,#1219);
#926=LINE('',#5688,#1220);
#927=LINE('',#5691,#1221);
#928=LINE('',#5693,#1222);
#929=LINE('',#5694,#1223);
#930=LINE('',#5697,#1224);
#931=LINE('',#5699,#1225);
#932=LINE('',#5700,#1226);
#933=LINE('',#5702,#1227);
#934=LINE('',#5705,#1228);
#935=LINE('',#5707,#1229);
#936=LINE('',#5709,#1230);
#937=LINE('',#5711,#1231);
#938=LINE('',#5712,#1232);
#939=LINE('',#5719,#1233);
#940=LINE('',#5721,#1234);
#941=LINE('',#5722,#1235);
#942=LINE('',#5725,#1236);
#943=LINE('',#5727,#1237);
#944=LINE('',#5728,#1238);
#945=LINE('',#5734,#1239);
#946=LINE('',#5736,#1240);
#947=LINE('',#5738,#1241);
#948=LINE('',#5740,#1242);
#949=LINE('',#5746,#1243);
#950=LINE('',#5748,#1244);
#951=LINE('',#5750,#1245);
#952=LINE('',#5751,#1246);
#953=LINE('',#5754,#1247);
#954=LINE('',#5756,#1248);
#955=LINE('',#5757,#1249);
#956=LINE('',#5760,#1250);
#957=LINE('',#5762,#1251);
#958=LINE('',#5763,#1252);
#959=LINE('',#5765,#1253);
#960=LINE('',#5768,#1254);
#961=LINE('',#5770,#1255);
#962=LINE('',#5772,#1256);
#963=LINE('',#5774,#1257);
#964=LINE('',#5775,#1258);
#965=LINE('',#5780,#1259);
#966=LINE('',#5785,#1260);
#967=LINE('',#5787,#1261);
#968=LINE('',#5789,#1262);
#969=LINE('',#5790,#1263);
#970=LINE('',#5794,#1264);
#971=LINE('',#5796,#1265);
#972=LINE('',#5798,#1266);
#973=LINE('',#5799,#1267);
#974=LINE('',#5801,#1268);
#975=LINE('',#5802,#1269);
#976=LINE('',#5805,#1270);
#977=LINE('',#5807,#1271);
#978=LINE('',#5809,#1272);
#979=LINE('',#5811,#1273);
#980=LINE('',#5812,#1274);
#981=LINE('',#5816,#1275);
#982=LINE('',#5818,#1276);
#983=LINE('',#5820,#1277);
#984=LINE('',#5821,#1278);
#985=LINE('',#5824,#1279);
#986=LINE('',#5826,#1280);
#987=LINE('',#5827,#1281);
#988=LINE('',#5829,#1282);
#989=LINE('',#5830,#1283);
#990=LINE('',#5836,#1284);
#991=LINE('',#5838,#1285);
#992=LINE('',#5840,#1286);
#993=LINE('',#5841,#1287);
#994=LINE('',#5848,#1288);
#995=LINE('',#5849,#1289);
#996=LINE('',#5850,#1290);
#997=LINE('',#5854,#1291);
#998=LINE('',#5855,#1292);
#999=LINE('',#5856,#1293);
#1000=LINE('',#5859,#1294);
#1001=LINE('',#5862,#1295);
#1002=LINE('',#5863,#1296);
#1003=LINE('',#5865,#1297);
#1004=LINE('',#5867,#1298);
#1005=LINE('',#5873,#1299);
#1006=LINE('',#5875,#1300);
#1007=LINE('',#5877,#1301);
#1008=LINE('',#5878,#1302);
#1009=LINE('',#5881,#1303);
#1010=LINE('',#5883,#1304);
#1011=LINE('',#5884,#1305);
#1012=LINE('',#5887,#1306);
#1013=LINE('',#5889,#1307);
#1014=LINE('',#5890,#1308);
#1015=LINE('',#5892,#1309);
#1016=LINE('',#5895,#1310);
#1017=LINE('',#5897,#1311);
#1018=LINE('',#5899,#1312);
#1019=LINE('',#5901,#1313);
#1020=LINE('',#5902,#1314);
#1021=LINE('',#5905,#1315);
#1022=LINE('',#5907,#1316);
#1023=LINE('',#5908,#1317);
#1024=LINE('',#5915,#1318);
#1025=LINE('',#5916,#1319);
#1026=LINE('',#5919,#1320);
#1027=LINE('',#5920,#1321);
#1028=LINE('',#5926,#1322);
#1029=LINE('',#5928,#1323);
#1030=LINE('',#5930,#1324);
#1031=LINE('',#5936,#1325);
#1032=LINE('',#5938,#1326);
#1033=LINE('',#5940,#1327);
#1034=LINE('',#5941,#1328);
#1035=LINE('',#5944,#1329);
#1036=LINE('',#5946,#1330);
#1037=LINE('',#5947,#1331);
#1038=LINE('',#5950,#1332);
#1039=LINE('',#5952,#1333);
#1040=LINE('',#5953,#1334);
#1041=LINE('',#5955,#1335);
#1042=LINE('',#5958,#1336);
#1043=LINE('',#5960,#1337);
#1044=LINE('',#5962,#1338);
#1045=LINE('',#5964,#1339);
#1046=LINE('',#5965,#1340);
#1047=LINE('',#5969,#1341);
#1048=LINE('',#5971,#1342);
#1049=LINE('',#5973,#1343);
#1050=LINE('',#5974,#1344);
#1051=LINE('',#5977,#1345);
#1052=LINE('',#5979,#1346);
#1053=LINE('',#5980,#1347);
#1054=LINE('',#5985,#1348);
#1055=LINE('',#5989,#1349);
#1056=LINE('',#5993,#1350);
#1057=LINE('',#5995,#1351);
#1058=LINE('',#5997,#1352);
#1059=LINE('',#5999,#1353);
#1060=LINE('',#6001,#1354);
#1061=LINE('',#6004,#1355);
#1062=LINE('',#6005,#1356);
#1063=LINE('',#6010,#1357);
#1064=LINE('',#6012,#1358);
#1065=LINE('',#6014,#1359);
#1066=LINE('',#6016,#1360);
#1067=LINE('',#6017,#1361);
#1068=LINE('',#6021,#1362);
#1069=LINE('',#6027,#1363);
#1070=LINE('',#6029,#1364);
#1071=LINE('',#6031,#1365);
#1072=LINE('',#6032,#1366);
#1073=LINE('',#6034,#1367);
#1074=LINE('',#6035,#1368);
#1075=LINE('',#6037,#1369);
#1076=LINE('',#6039,#1370);
#1077=LINE('',#6042,#1371);
#1078=LINE('',#6046,#1372);
#1079=LINE('',#6048,#1373);
#1080=LINE('',#6049,#1374);
#1081=LINE('',#6051,#1375);
#1082=LINE('',#6053,#1376);
#1083=LINE('',#6057,#1377);
#1084=LINE('',#6059,#1378);
#1085=LINE('',#6941,#1379);
#1086=LINE('',#6943,#1380);
#1087=LINE('',#6945,#1381);
#1088=LINE('',#6946,#1382);
#1089=LINE('',#6949,#1383);
#1090=LINE('',#6951,#1384);
#1091=LINE('',#6952,#1385);
#1092=LINE('',#6955,#1386);
#1093=LINE('',#6957,#1387);
#1094=LINE('',#6958,#1388);
#1095=LINE('',#6960,#1389);
#1096=LINE('',#6961,#1390);
#1097=LINE('',#6965,#1391);
#1098=LINE('',#6967,#1392);
#1099=LINE('',#6969,#1393);
#1100=LINE('',#6970,#1394);
#1101=LINE('',#6973,#1395);
#1102=LINE('',#6975,#1396);
#1103=LINE('',#6976,#1397);
#1104=LINE('',#6979,#1398);
#1105=LINE('',#6980,#1399);
#1106=LINE('',#6984,#1400);
#1107=LINE('',#6986,#1401);
#1108=LINE('',#6988,#1402);
#1109=LINE('',#6989,#1403);
#1110=LINE('',#6992,#1404);
#1111=LINE('',#6994,#1405);
#1112=LINE('',#6995,#1406);
#1113=LINE('',#6998,#1407);
#1114=LINE('',#7000,#1408);
#1115=LINE('',#7001,#1409);
#1116=LINE('',#7003,#1410);
#1117=LINE('',#7004,#1411);
#1118=LINE('',#7008,#1412);
#1119=LINE('',#7009,#1413);
#1120=LINE('',#7011,#1414);
#1121=VECTOR('',#3898,10.);
#1122=VECTOR('',#3905,10.);
#1123=VECTOR('',#3910,10.);
#1124=VECTOR('',#3915,10.);
#1125=VECTOR('',#3918,10.);
#1126=VECTOR('',#3923,10.);
#1127=VECTOR('',#3930,10.);
#1128=VECTOR('',#3935,10.);
#1129=VECTOR('',#3940,10.);
#1130=VECTOR('',#3943,10.);
#1131=VECTOR('',#3948,10.);
#1132=VECTOR('',#3951,10.);
#1133=VECTOR('',#3958,10.);
#1134=VECTOR('',#3963,10.);
#1135=VECTOR('',#3970,10.);
#1136=VECTOR('',#3975,10.);
#1137=VECTOR('',#3980,10.);
#1138=VECTOR('',#3985,10.);
#1139=VECTOR('',#3992,10.);
#1140=VECTOR('',#3997,10.);
#1141=VECTOR('',#4016,2.17846096908266);
#1142=VECTOR('',#4021,2.33923048454133);
#1143=VECTOR('',#4026,2.5);
#1144=VECTOR('',#4039,5.05813690328693);
#1145=VECTOR('',#4044,10.);
#1146=VECTOR('',#4051,10.);
#1147=VECTOR('',#4056,10.);
#1148=VECTOR('',#4061,10.);
#1149=VECTOR('',#4064,10.);
#1150=VECTOR('',#4069,10.);
#1151=VECTOR('',#4076,10.);
#1152=VECTOR('',#4081,10.);
#1153=VECTOR('',#4086,10.);
#1154=VECTOR('',#4089,10.);
#1155=VECTOR('',#4094,10.);
#1156=VECTOR('',#4097,10.);
#1157=VECTOR('',#4104,10.);
#1158=VECTOR('',#4109,10.);
#1159=VECTOR('',#4116,10.);
#1160=VECTOR('',#4121,10.);
#1161=VECTOR('',#4126,10.);
#1162=VECTOR('',#4131,10.);
#1163=VECTOR('',#4138,10.);
#1164=VECTOR('',#4143,10.);
#1165=VECTOR('',#4162,2.17846096908266);
#1166=VECTOR('',#4167,2.33923048454133);
#1167=VECTOR('',#4172,2.5);
#1168=VECTOR('',#4185,5.05813690328693);
#1169=VECTOR('',#4190,10.);
#1170=VECTOR('',#4197,10.);
#1171=VECTOR('',#4202,10.);
#1172=VECTOR('',#4207,10.);
#1173=VECTOR('',#4210,10.);
#1174=VECTOR('',#4215,10.);
#1175=VECTOR('',#4222,10.);
#1176=VECTOR('',#4227,10.);
#1177=VECTOR('',#4232,10.);
#1178=VECTOR('',#4235,10.);
#1179=VECTOR('',#4240,10.);
#1180=VECTOR('',#4243,10.);
#1181=VECTOR('',#4250,10.);
#1182=VECTOR('',#4255,10.);
#1183=VECTOR('',#4262,10.);
#1184=VECTOR('',#4267,10.);
#1185=VECTOR('',#4272,10.);
#1186=VECTOR('',#4277,10.);
#1187=VECTOR('',#4284,10.);
#1188=VECTOR('',#4289,10.);
#1189=VECTOR('',#4308,2.17846096908266);
#1190=VECTOR('',#4313,2.33923048454133);
#1191=VECTOR('',#4318,2.5);
#1192=VECTOR('',#4331,5.05813690328693);
#1193=VECTOR('',#4336,10.);
#1194=VECTOR('',#4343,10.);
#1195=VECTOR('',#4348,10.);
#1196=VECTOR('',#4353,10.);
#1197=VECTOR('',#4356,10.);
#1198=VECTOR('',#4361,10.);
#1199=VECTOR('',#4368,10.);
#1200=VECTOR('',#4373,10.);
#1201=VECTOR('',#4378,10.);
#1202=VECTOR('',#4381,10.);
#1203=VECTOR('',#4386,10.);
#1204=VECTOR('',#4389,10.);
#1205=VECTOR('',#4396,10.);
#1206=VECTOR('',#4401,10.);
#1207=VECTOR('',#4408,10.);
#1208=VECTOR('',#4413,10.);
#1209=VECTOR('',#4418,10.);
#1210=VECTOR('',#4423,10.);
#1211=VECTOR('',#4430,10.);
#1212=VECTOR('',#4435,10.);
#1213=VECTOR('',#4454,2.17846096908266);
#1214=VECTOR('',#4459,2.33923048454133);
#1215=VECTOR('',#4464,2.5);
#1216=VECTOR('',#4477,5.05813690328693);
#1217=VECTOR('',#4482,10.);
#1218=VECTOR('',#4483,10.);
#1219=VECTOR('',#4484,10.);
#1220=VECTOR('',#4485,10.);
#1221=VECTOR('',#4488,10.);
#1222=VECTOR('',#4489,10.);
#1223=VECTOR('',#4490,10.);
#1224=VECTOR('',#4493,10.);
#1225=VECTOR('',#4494,10.);
#1226=VECTOR('',#4495,10.);
#1227=VECTOR('',#4498,10.);
#1228=VECTOR('',#4501,10.);
#1229=VECTOR('',#4502,10.);
#1230=VECTOR('',#4503,10.);
#1231=VECTOR('',#4504,10.);
#1232=VECTOR('',#4505,10.);
#1233=VECTOR('',#4512,10.);
#1234=VECTOR('',#4513,10.);
#1235=VECTOR('',#4514,10.);
#1236=VECTOR('',#4517,10.);
#1237=VECTOR('',#4518,10.);
#1238=VECTOR('',#4519,10.);
#1239=VECTOR('',#4526,10.);
#1240=VECTOR('',#4529,10.);
#1241=VECTOR('',#4532,3.25);
#1242=VECTOR('',#4535,3.25);
#1243=VECTOR('',#4542,10.);
#1244=VECTOR('',#4543,10.);
#1245=VECTOR('',#4544,10.);
#1246=VECTOR('',#4545,10.);
#1247=VECTOR('',#4548,10.);
#1248=VECTOR('',#4549,10.);
#1249=VECTOR('',#4550,10.);
#1250=VECTOR('',#4553,10.);
#1251=VECTOR('',#4554,10.);
#1252=VECTOR('',#4555,10.);
#1253=VECTOR('',#4558,10.);
#1254=VECTOR('',#4561,10.);
#1255=VECTOR('',#4562,10.);
#1256=VECTOR('',#4563,10.);
#1257=VECTOR('',#4564,10.);
#1258=VECTOR('',#4565,10.);
#1259=VECTOR('',#4570,2.5);
#1260=VECTOR('',#4575,10.);
#1261=VECTOR('',#4576,10.);
#1262=VECTOR('',#4577,10.);
#1263=VECTOR('',#4578,10.);
#1264=VECTOR('',#4581,10.);
#1265=VECTOR('',#4582,10.);
#1266=VECTOR('',#4583,10.);
#1267=VECTOR('',#4584,10.);
#1268=VECTOR('',#4587,10.);
#1269=VECTOR('',#4588,10.);
#1270=VECTOR('',#4591,10.);
#1271=VECTOR('',#4592,10.);
#1272=VECTOR('',#4593,10.);
#1273=VECTOR('',#4594,10.);
#1274=VECTOR('',#4595,10.);
#1275=VECTOR('',#4598,10.);
#1276=VECTOR('',#4599,10.);
#1277=VECTOR('',#4600,10.);
#1278=VECTOR('',#4601,10.);
#1279=VECTOR('',#4604,10.);
#1280=VECTOR('',#4605,10.);
#1281=VECTOR('',#4606,10.);
#1282=VECTOR('',#4609,10.);
#1283=VECTOR('',#4610,10.);
#1284=VECTOR('',#4617,10.);
#1285=VECTOR('',#4618,10.);
#1286=VECTOR('',#4619,10.);
#1287=VECTOR('',#4620,10.);
#1288=VECTOR('',#4629,10.);
#1289=VECTOR('',#4630,10.);
#1290=VECTOR('',#4631,10.);
#1291=VECTOR('',#4634,10.);
#1292=VECTOR('',#4635,10.);
#1293=VECTOR('',#4636,10.);
#1294=VECTOR('',#4641,10.);
#1295=VECTOR('',#4644,10.);
#1296=VECTOR('',#4645,10.);
#1297=VECTOR('',#4648,10.);
#1298=VECTOR('',#4651,10.);
#1299=VECTOR('',#4658,10.);
#1300=VECTOR('',#4659,10.);
#1301=VECTOR('',#4660,10.);
#1302=VECTOR('',#4661,10.);
#1303=VECTOR('',#4664,10.);
#1304=VECTOR('',#4665,10.);
#1305=VECTOR('',#4666,10.);
#1306=VECTOR('',#4669,10.);
#1307=VECTOR('',#4670,10.);
#1308=VECTOR('',#4671,10.);
#1309=VECTOR('',#4674,10.);
#1310=VECTOR('',#4677,10.);
#1311=VECTOR('',#4678,10.);
#1312=VECTOR('',#4679,10.);
#1313=VECTOR('',#4680,10.);
#1314=VECTOR('',#4681,10.);
#1315=VECTOR('',#4684,10.);
#1316=VECTOR('',#4685,10.);
#1317=VECTOR('',#4686,10.);
#1318=VECTOR('',#4693,10.);
#1319=VECTOR('',#4694,10.);
#1320=VECTOR('',#4697,10.);
#1321=VECTOR('',#4698,10.);
#1322=VECTOR('',#4705,10.);
#1323=VECTOR('',#4708,3.25);
#1324=VECTOR('',#4711,3.25);
#1325=VECTOR('',#4718,10.);
#1326=VECTOR('',#4719,10.);
#1327=VECTOR('',#4720,10.);
#1328=VECTOR('',#4721,10.);
#1329=VECTOR('',#4724,10.);
#1330=VECTOR('',#4725,10.);
#1331=VECTOR('',#4726,10.);
#1332=VECTOR('',#4729,10.);
#1333=VECTOR('',#4730,10.);
#1334=VECTOR('',#4731,10.);
#1335=VECTOR('',#4734,10.);
#1336=VECTOR('',#4737,10.);
#1337=VECTOR('',#4738,10.);
#1338=VECTOR('',#4739,10.);
#1339=VECTOR('',#4740,10.);
#1340=VECTOR('',#4741,10.);
#1341=VECTOR('',#4744,10.);
#1342=VECTOR('',#4745,10.);
#1343=VECTOR('',#4746,10.);
#1344=VECTOR('',#4747,10.);
#1345=VECTOR('',#4750,10.);
#1346=VECTOR('',#4751,10.);
#1347=VECTOR('',#4752,10.);
#1348=VECTOR('',#4757,10.);
#1349=VECTOR('',#4762,10.);
#1350=VECTOR('',#4765,10.);
#1351=VECTOR('',#4766,10.);
#1352=VECTOR('',#4767,10.);
#1353=VECTOR('',#4768,10.);
#1354=VECTOR('',#4771,10.);
#1355=VECTOR('',#4774,10.);
#1356=VECTOR('',#4775,10.);
#1357=VECTOR('',#4780,10.);
#1358=VECTOR('',#4781,10.);
#1359=VECTOR('',#4782,10.);
#1360=VECTOR('',#4783,10.);
#1361=VECTOR('',#4784,10.);
#1362=VECTOR('',#4787,10.);
#1363=VECTOR('',#4794,10.);
#1364=VECTOR('',#4795,10.);
#1365=VECTOR('',#4796,10.);
#1366=VECTOR('',#4797,10.);
#1367=VECTOR('',#4800,10.);
#1368=VECTOR('',#4801,10.);
#1369=VECTOR('',#4804,10.);
#1370=VECTOR('',#4807,10.);
#1371=VECTOR('',#4810,10.);
#1372=VECTOR('',#4815,10.);
#1373=VECTOR('',#4816,10.);
#1374=VECTOR('',#4817,10.);
#1375=VECTOR('',#4820,10.);
#1376=VECTOR('',#4823,10.);
#1377=VECTOR('',#4828,2.5);
#1378=VECTOR('',#4831,10.);
#1379=VECTOR('',#4848,10.);
#1380=VECTOR('',#4849,10.);
#1381=VECTOR('',#4850,10.);
#1382=VECTOR('',#4851,10.);
#1383=VECTOR('',#4854,10.);
#1384=VECTOR('',#4855,10.);
#1385=VECTOR('',#4856,10.);
#1386=VECTOR('',#4859,10.);
#1387=VECTOR('',#4860,10.);
#1388=VECTOR('',#4861,10.);
#1389=VECTOR('',#4864,10.);
#1390=VECTOR('',#4865,10.);
#1391=VECTOR('',#4868,10.);
#1392=VECTOR('',#4869,10.);
#1393=VECTOR('',#4870,10.);
#1394=VECTOR('',#4871,10.);
#1395=VECTOR('',#4874,10.);
#1396=VECTOR('',#4875,10.);
#1397=VECTOR('',#4876,10.);
#1398=VECTOR('',#4879,10.);
#1399=VECTOR('',#4880,10.);
#1400=VECTOR('',#4883,10.);
#1401=VECTOR('',#4884,10.);
#1402=VECTOR('',#4885,10.);
#1403=VECTOR('',#4886,10.);
#1404=VECTOR('',#4889,10.);
#1405=VECTOR('',#4890,10.);
#1406=VECTOR('',#4891,10.);
#1407=VECTOR('',#4894,10.);
#1408=VECTOR('',#4895,10.);
#1409=VECTOR('',#4896,10.);
#1410=VECTOR('',#4899,10.);
#1411=VECTOR('',#4900,10.);
#1412=VECTOR('',#4905,10.);
#1413=VECTOR('',#4906,10.);
#1414=VECTOR('',#4909,10.);
#1415=B_SPLINE_CURVE_WITH_KNOTS('',3,(#4939,#4940,#4941,#4942,#4943,#4944,
#4945,#4946,#4947,#4948,#4949,#4950,#4951,#4952,#4953),.UNSPECIFIED.,.F.,
 .F.,(4,2,2,3,2,2,4),(-0.0714521071173775,-0.0712222400952786,-0.0356111200476392,
0.,0.0356111200476392,0.0712222400952784,0.0714521071173274),
 .UNSPECIFIED.);
#1416=B_SPLINE_CURVE_WITH_KNOTS('',3,(#4981,#4982,#4983,#4984,#4985,#4986,
#4987,#4988,#4989,#4990,#4991,#4992,#4993,#4994,#4995),.UNSPECIFIED.,.F.,
 .F.,(4,2,2,3,2,2,4),(-0.071452107117379,-0.0712222400952786,-0.0356111200476392,
0.,0.0356111200476392,0.0712222400952784,0.071452107117329),
 .UNSPECIFIED.);
#1417=B_SPLINE_CURVE_WITH_KNOTS('',3,(#5020,#5021,#5022,#5023,#5024,#5025,
#5026,#5027,#5028,#5029,#5030,#5031,#5032,#5033,#5034),.UNSPECIFIED.,.F.,
 .F.,(4,2,2,3,2,2,4),(-0.0714521071173781,-0.0712222400952784,-0.0356111200476392,
0.,0.0356111200476392,0.0712222400952785,0.0714521071173282),
 .UNSPECIFIED.);
#1418=B_SPLINE_CURVE_WITH_KNOTS('',3,(#5050,#5051,#5052,#5053,#5054,#5055,
#5056,#5057,#5058,#5059,#5060,#5061,#5062,#5063,#5064),.UNSPECIFIED.,.F.,
 .F.,(4,2,2,3,2,2,4),(-0.0714521071173768,-0.0712222400952786,-0.0356111200476392,
0.,0.0356111200476392,0.0712222400952785,0.0714521071173268),
 .UNSPECIFIED.);
#1419=B_SPLINE_CURVE_WITH_KNOTS('',3,(#5125,#5126,#5127,#5128,#5129,#5130,
#5131,#5132,#5133,#5134,#5135,#5136,#5137,#5138,#5139),.UNSPECIFIED.,.F.,
 .F.,(4,2,2,3,2,2,4),(-0.0714521071173775,-0.0712222400952786,-0.0356111200476392,
0.,0.0356111200476392,0.0712222400952784,0.0714521071173274),
 .UNSPECIFIED.);
#1420=B_SPLINE_CURVE_WITH_KNOTS('',3,(#5167,#5168,#5169,#5170,#5171,#5172,
#5173,#5174,#5175,#5176,#5177,#5178,#5179,#5180,#5181),.UNSPECIFIED.,.F.,
 .F.,(4,2,2,3,2,2,4),(-0.071452107117379,-0.0712222400952786,-0.0356111200476392,
0.,0.0356111200476392,0.0712222400952784,0.071452107117329),
 .UNSPECIFIED.);
#1421=B_SPLINE_CURVE_WITH_KNOTS('',3,(#5206,#5207,#5208,#5209,#5210,#5211,
#5212,#5213,#5214,#5215,#5216,#5217,#5218,#5219,#5220),.UNSPECIFIED.,.F.,
 .F.,(4,2,2,3,2,2,4),(-0.0714521071173781,-0.0712222400952784,-0.0356111200476392,
0.,0.0356111200476392,0.0712222400952785,0.0714521071173282),
 .UNSPECIFIED.);
#1422=B_SPLINE_CURVE_WITH_KNOTS('',3,(#5236,#5237,#5238,#5239,#5240,#5241,
#5242,#5243,#5244,#5245,#5246,#5247,#5248,#5249,#5250),.UNSPECIFIED.,.F.,
 .F.,(4,2,2,3,2,2,4),(-0.0714521071173768,-0.0712222400952786,-0.0356111200476392,
0.,0.0356111200476392,0.0712222400952785,0.0714521071173268),
 .UNSPECIFIED.);
#1423=B_SPLINE_CURVE_WITH_KNOTS('',3,(#5311,#5312,#5313,#5314,#5315,#5316,
#5317,#5318,#5319,#5320,#5321,#5322,#5323,#5324,#5325),.UNSPECIFIED.,.F.,
 .F.,(4,2,2,3,2,2,4),(-0.0714521071173775,-0.0712222400952786,-0.0356111200476392,
0.,0.0356111200476392,0.0712222400952784,0.0714521071173274),
 .UNSPECIFIED.);
#1424=B_SPLINE_CURVE_WITH_KNOTS('',3,(#5353,#5354,#5355,#5356,#5357,#5358,
#5359,#5360,#5361,#5362,#5363,#5364,#5365,#5366,#5367),.UNSPECIFIED.,.F.,
 .F.,(4,2,2,3,2,2,4),(-0.071452107117379,-0.0712222400952786,-0.0356111200476392,
0.,0.0356111200476392,0.0712222400952784,0.071452107117329),
 .UNSPECIFIED.);
#1425=B_SPLINE_CURVE_WITH_KNOTS('',3,(#5392,#5393,#5394,#5395,#5396,#5397,
#5398,#5399,#5400,#5401,#5402,#5403,#5404,#5405,#5406),.UNSPECIFIED.,.F.,
 .F.,(4,2,2,3,2,2,4),(-0.0714521071173781,-0.0712222400952784,-0.0356111200476392,
0.,0.0356111200476392,0.0712222400952785,0.0714521071173282),
 .UNSPECIFIED.);
#1426=B_SPLINE_CURVE_WITH_KNOTS('',3,(#5422,#5423,#5424,#5425,#5426,#5427,
#5428,#5429,#5430,#5431,#5432,#5433,#5434,#5435,#5436),.UNSPECIFIED.,.F.,
 .F.,(4,2,2,3,2,2,4),(-0.0714521071173768,-0.0712222400952786,-0.0356111200476392,
0.,0.0356111200476392,0.0712222400952785,0.0714521071173268),
 .UNSPECIFIED.);
#1427=B_SPLINE_CURVE_WITH_KNOTS('',3,(#5497,#5498,#5499,#5500,#5501,#5502,
#5503,#5504,#5505,#5506,#5507,#5508,#5509,#5510,#5511),.UNSPECIFIED.,.F.,
 .F.,(4,2,2,3,2,2,4),(-0.0714521071173775,-0.0712222400952786,-0.0356111200476392,
0.,0.0356111200476392,0.0712222400952784,0.0714521071173274),
 .UNSPECIFIED.);
#1428=B_SPLINE_CURVE_WITH_KNOTS('',3,(#5539,#5540,#5541,#5542,#5543,#5544,
#5545,#5546,#5547,#5548,#5549,#5550,#5551,#5552,#5553),.UNSPECIFIED.,.F.,
 .F.,(4,2,2,3,2,2,4),(-0.071452107117379,-0.0712222400952786,-0.0356111200476392,
0.,0.0356111200476392,0.0712222400952784,0.071452107117329),
 .UNSPECIFIED.);
#1429=B_SPLINE_CURVE_WITH_KNOTS('',3,(#5578,#5579,#5580,#5581,#5582,#5583,
#5584,#5585,#5586,#5587,#5588,#5589,#5590,#5591,#5592),.UNSPECIFIED.,.F.,
 .F.,(4,2,2,3,2,2,4),(-0.0714521071173781,-0.0712222400952784,-0.0356111200476392,
0.,0.0356111200476392,0.0712222400952785,0.0714521071173282),
 .UNSPECIFIED.);
#1430=B_SPLINE_CURVE_WITH_KNOTS('',3,(#5608,#5609,#5610,#5611,#5612,#5613,
#5614,#5615,#5616,#5617,#5618,#5619,#5620,#5621,#5622),.UNSPECIFIED.,.F.,
 .F.,(4,2,2,3,2,2,4),(-0.0714521071173768,-0.0712222400952786,-0.0356111200476392,
0.,0.0356111200476392,0.0712222400952785,0.0714521071173268),
 .UNSPECIFIED.);
#1431=B_SPLINE_CURVE_WITH_KNOTS('',3,(#6855,#6856,#6857,#6858,#6859,#6860,
#6861,#6862,#6863,#6864,#6865,#6866,#6867,#6868,#6869,#6870,#6871,#6872,
#6873,#6874,#6875,#6876,#6877,#6878,#6879,#6880,#6881,#6882,#6883,#6884,
#6885,#6886,#6887,#6888,#6889,#6890,#6891,#6892,#6893,#6894,#6895,#6896,
#6897,#6898,#6899,#6900,#6901,#6902,#6903,#6904,#6905,#6906,#6907,#6908,
#6909,#6910,#6911,#6912,#6913,#6914,#6915,#6916,#6917,#6918,#6919,#6920,
#6921,#6922,#6923,#6924,#6925,#6926,#6927,#6928,#6929,#6930,#6931,#6932,
#6933),.UNSPECIFIED.,.F.,.F.,(4,1,1,1,1,1,1,1,1,1,1,1,1,1,1,1,1,1,1,1,1,
1,1,1,1,1,1,1,1,1,1,1,1,1,1,1,1,1,1,1,1,1,1,1,1,1,1,1,1,1,1,1,1,1,1,1,1,
1,1,1,1,1,1,1,1,1,1,1,1,1,1,1,1,1,1,1,4),(0.,0.496040945303652,0.992081890607303,
1.48812283591095,1.98416378121461,2.48020472651826,2.97624567182191,3.47228661712556,
3.96832756242921,4.46436850773286,4.96040945303652,5.45645039834017,5.95249134364382,
6.44853228894747,6.94457323425112,7.44061417955477,7.93665512485842,8.43269607016208,
8.92873701546573,9.42477796076938,9.92081890607303,10.4168598513767,10.9129007966803,
11.408941741984,11.9049826872876,12.4010236325913,12.8970645778949,13.3931055231986,
13.8891464685022,14.3851874138059,14.8812283591095,15.3772693044132,15.8733102497168,
16.3693511950205,16.8653921403242,17.3614330856278,17.8574740309315,18.3535149762351,
18.8495559215388,19.3455968668424,19.8416378121461,20.3376787574497,20.8337197027534,
21.329760648057,21.8258015933607,22.3218425386643,22.817883483968,23.3139244292716,
23.8099653745753,24.3060063198789,24.8020472651826,25.2980882104862,25.7941291557899,
26.2901701010935,26.7862110463972,27.2822519917008,27.7782929370045,28.2743338823081,
28.7703748276118,29.2664157729154,29.7624567182191,30.2584976635227,30.7545386088264,
31.25057955413,31.7466204994337,32.2426614447374,32.738702390041,33.2347433353447,
33.7307842806483,34.226825225952,34.7228661712556,35.2189071165593,35.7149480618629,
36.2109890071666,36.7070299524702,37.2030708977739,37.6991118430775),
 .UNSPECIFIED.);
#1432=VERTEX_POINT('',#4937);
#1433=VERTEX_POINT('',#4938);
#1434=VERTEX_POINT('',#4954);
#1435=VERTEX_POINT('',#4956);
#1436=VERTEX_POINT('',#4958);
#1437=VERTEX_POINT('',#4960);
#1438=VERTEX_POINT('',#4964);
#1439=VERTEX_POINT('',#4968);
#1440=VERTEX_POINT('',#4970);
#1441=VERTEX_POINT('',#4972);
#1442=VERTEX_POINT('',#4976);
#1443=VERTEX_POINT('',#4980);
#1444=VERTEX_POINT('',#4996);
#1445=VERTEX_POINT('',#4998);
#1446=VERTEX_POINT('',#5002);
#1447=VERTEX_POINT('',#5006);
#1448=VERTEX_POINT('',#5008);
#1449=VERTEX_POINT('',#5010);
#1450=VERTEX_POINT('',#5014);
#1451=VERTEX_POINT('',#5018);
#1452=VERTEX_POINT('',#5019);
#1453=VERTEX_POINT('',#5035);
#1454=VERTEX_POINT('',#5037);
#1455=VERTEX_POINT('',#5039);
#1456=VERTEX_POINT('',#5041);
#1457=VERTEX_POINT('',#5045);
#1458=VERTEX_POINT('',#5049);
#1459=VERTEX_POINT('',#5065);
#1460=VERTEX_POINT('',#5067);
#1461=VERTEX_POINT('',#5071);
#1462=VERTEX_POINT('',#5075);
#1463=VERTEX_POINT('',#5079);
#1464=VERTEX_POINT('',#5084);
#1465=VERTEX_POINT('',#5092);
#1466=VERTEX_POINT('',#5094);
#1467=VERTEX_POINT('',#5098);
#1468=VERTEX_POINT('',#5101);
#1469=VERTEX_POINT('',#5105);
#1470=VERTEX_POINT('',#5109);
#1471=VERTEX_POINT('',#5114);
#1472=VERTEX_POINT('',#5116);
#1473=VERTEX_POINT('',#5123);
#1474=VERTEX_POINT('',#5124);
#1475=VERTEX_POINT('',#5140);
#1476=VERTEX_POINT('',#5142);
#1477=VERTEX_POINT('',#5144);
#1478=VERTEX_POINT('',#5146);
#1479=VERTEX_POINT('',#5150);
#1480=VERTEX_POINT('',#5154);
#1481=VERTEX_POINT('',#5156);
#1482=VERTEX_POINT('',#5158);
#1483=VERTEX_POINT('',#5162);
#1484=VERTEX_POINT('',#5166);
#1485=VERTEX_POINT('',#5182);
#1486=VERTEX_POINT('',#5184);
#1487=VERTEX_POINT('',#5188);
#1488=VERTEX_POINT('',#5192);
#1489=VERTEX_POINT('',#5194);
#1490=VERTEX_POINT('',#5196);
#1491=VERTEX_POINT('',#5200);
#1492=VERTEX_POINT('',#5204);
#1493=VERTEX_POINT('',#5205);
#1494=VERTEX_POINT('',#5221);
#1495=VERTEX_POINT('',#5223);
#1496=VERTEX_POINT('',#5225);
#1497=VERTEX_POINT('',#5227);
#1498=VERTEX_POINT('',#5231);
#1499=VERTEX_POINT('',#5235);
#1500=VERTEX_POINT('',#5251);
#1501=VERTEX_POINT('',#5253);
#1502=VERTEX_POINT('',#5257);
#1503=VERTEX_POINT('',#5261);
#1504=VERTEX_POINT('',#5265);
#1505=VERTEX_POINT('',#5270);
#1506=VERTEX_POINT('',#5278);
#1507=VERTEX_POINT('',#5280);
#1508=VERTEX_POINT('',#5284);
#1509=VERTEX_POINT('',#5287);
#1510=VERTEX_POINT('',#5291);
#1511=VERTEX_POINT('',#5295);
#1512=VERTEX_POINT('',#5300);
#1513=VERTEX_POINT('',#5302);
#1514=VERTEX_POINT('',#5309);
#1515=VERTEX_POINT('',#5310);
#1516=VERTEX_POINT('',#5326);
#1517=VERTEX_POINT('',#5328);
#1518=VERTEX_POINT('',#5330);
#1519=VERTEX_POINT('',#5332);
#1520=VERTEX_POINT('',#5336);
#1521=VERTEX_POINT('',#5340);
#1522=VERTEX_POINT('',#5342);
#1523=VERTEX_POINT('',#5344);
#1524=VERTEX_POINT('',#5348);
#1525=VERTEX_POINT('',#5352);
#1526=VERTEX_POINT('',#5368);
#1527=VERTEX_POINT('',#5370);
#1528=VERTEX_POINT('',#5374);
#1529=VERTEX_POINT('',#5378);
#1530=VERTEX_POINT('',#5380);
#1531=VERTEX_POINT('',#5382);
#1532=VERTEX_POINT('',#5386);
#1533=VERTEX_POINT('',#5390);
#1534=VERTEX_POINT('',#5391);
#1535=VERTEX_POINT('',#5407);
#1536=VERTEX_POINT('',#5409);
#1537=VERTEX_POINT('',#5411);
#1538=VERTEX_POINT('',#5413);
#1539=VERTEX_POINT('',#5417);
#1540=VERTEX_POINT('',#5421);
#1541=VERTEX_POINT('',#5437);
#1542=VERTEX_POINT('',#5439);
#1543=VERTEX_POINT('',#5443);
#1544=VERTEX_POINT('',#5447);
#1545=VERTEX_POINT('',#5451);
#1546=VERTEX_POINT('',#5456);
#1547=VERTEX_POINT('',#5464);
#1548=VERTEX_POINT('',#5466);
#1549=VERTEX_POINT('',#5470);
#1550=VERTEX_POINT('',#5473);
#1551=VERTEX_POINT('',#5477);
#1552=VERTEX_POINT('',#5481);
#1553=VERTEX_POINT('',#5486);
#1554=VERTEX_POINT('',#5488);
#1555=VERTEX_POINT('',#5495);
#1556=VERTEX_POINT('',#5496);
#1557=VERTEX_POINT('',#5512);
#1558=VERTEX_POINT('',#5514);
#1559=VERTEX_POINT('',#5516);
#1560=VERTEX_POINT('',#5518);
#1561=VERTEX_POINT('',#5522);
#1562=VERTEX_POINT('',#5526);
#1563=VERTEX_POINT('',#5528);
#1564=VERTEX_POINT('',#5530);
#1565=VERTEX_POINT('',#5534);
#1566=VERTEX_POINT('',#5538);
#1567=VERTEX_POINT('',#5554);
#1568=VERTEX_POINT('',#5556);
#1569=VERTEX_POINT('',#5560);
#1570=VERTEX_POINT('',#5564);
#1571=VERTEX_POINT('',#5566);
#1572=VERTEX_POINT('',#5568);
#1573=VERTEX_POINT('',#5572);
#1574=VERTEX_POINT('',#5576);
#1575=VERTEX_POINT('',#5577);
#1576=VERTEX_POINT('',#5593);
#1577=VERTEX_POINT('',#5595);
#1578=VERTEX_POINT('',#5597);
#1579=VERTEX_POINT('',#5599);
#1580=VERTEX_POINT('',#5603);
#1581=VERTEX_POINT('',#5607);
#1582=VERTEX_POINT('',#5623);
#1583=VERTEX_POINT('',#5625);
#1584=VERTEX_POINT('',#5629);
#1585=VERTEX_POINT('',#5633);
#1586=VERTEX_POINT('',#5637);
#1587=VERTEX_POINT('',#5642);
#1588=VERTEX_POINT('',#5650);
#1589=VERTEX_POINT('',#5652);
#1590=VERTEX_POINT('',#5656);
#1591=VERTEX_POINT('',#5659);
#1592=VERTEX_POINT('',#5663);
#1593=VERTEX_POINT('',#5667);
#1594=VERTEX_POINT('',#5672);
#1595=VERTEX_POINT('',#5674);
#1596=VERTEX_POINT('',#5681);
#1597=VERTEX_POINT('',#5682);
#1598=VERTEX_POINT('',#5684);
#1599=VERTEX_POINT('',#5686);
#1600=VERTEX_POINT('',#5690);
#1601=VERTEX_POINT('',#5692);
#1602=VERTEX_POINT('',#5696);
#1603=VERTEX_POINT('',#5698);
#1604=VERTEX_POINT('',#5704);
#1605=VERTEX_POINT('',#5706);
#1606=VERTEX_POINT('',#5708);
#1607=VERTEX_POINT('',#5710);
#1608=VERTEX_POINT('',#5713);
#1609=VERTEX_POINT('',#5715);
#1610=VERTEX_POINT('',#5718);
#1611=VERTEX_POINT('',#5720);
#1612=VERTEX_POINT('',#5724);
#1613=VERTEX_POINT('',#5726);
#1614=VERTEX_POINT('',#5729);
#1615=VERTEX_POINT('',#5731);
#1616=VERTEX_POINT('',#5744);
#1617=VERTEX_POINT('',#5745);
#1618=VERTEX_POINT('',#5747);
#1619=VERTEX_POINT('',#5749);
#1620=VERTEX_POINT('',#5753);
#1621=VERTEX_POINT('',#5755);
#1622=VERTEX_POINT('',#5759);
#1623=VERTEX_POINT('',#5761);
#1624=VERTEX_POINT('',#5767);
#1625=VERTEX_POINT('',#5769);
#1626=VERTEX_POINT('',#5771);
#1627=VERTEX_POINT('',#5773);
#1628=VERTEX_POINT('',#5777);
#1629=VERTEX_POINT('',#5779);
#1630=VERTEX_POINT('',#5783);
#1631=VERTEX_POINT('',#5784);
#1632=VERTEX_POINT('',#5786);
#1633=VERTEX_POINT('',#5788);
#1634=VERTEX_POINT('',#5792);
#1635=VERTEX_POINT('',#5793);
#1636=VERTEX_POINT('',#5795);
#1637=VERTEX_POINT('',#5797);
#1638=VERTEX_POINT('',#5804);
#1639=VERTEX_POINT('',#5806);
#1640=VERTEX_POINT('',#5808);
#1641=VERTEX_POINT('',#5810);
#1642=VERTEX_POINT('',#5814);
#1643=VERTEX_POINT('',#5815);
#1644=VERTEX_POINT('',#5817);
#1645=VERTEX_POINT('',#5819);
#1646=VERTEX_POINT('',#5823);
#1647=VERTEX_POINT('',#5825);
#1648=VERTEX_POINT('',#5834);
#1649=VERTEX_POINT('',#5835);
#1650=VERTEX_POINT('',#5837);
#1651=VERTEX_POINT('',#5839);
#1652=VERTEX_POINT('',#5846);
#1653=VERTEX_POINT('',#5847);
#1654=VERTEX_POINT('',#5852);
#1655=VERTEX_POINT('',#5853);
#1656=VERTEX_POINT('',#5861);
#1657=VERTEX_POINT('',#5871);
#1658=VERTEX_POINT('',#5872);
#1659=VERTEX_POINT('',#5874);
#1660=VERTEX_POINT('',#5876);
#1661=VERTEX_POINT('',#5880);
#1662=VERTEX_POINT('',#5882);
#1663=VERTEX_POINT('',#5886);
#1664=VERTEX_POINT('',#5888);
#1665=VERTEX_POINT('',#5894);
#1666=VERTEX_POINT('',#5896);
#1667=VERTEX_POINT('',#5898);
#1668=VERTEX_POINT('',#5900);
#1669=VERTEX_POINT('',#5904);
#1670=VERTEX_POINT('',#5906);
#1671=VERTEX_POINT('',#5909);
#1672=VERTEX_POINT('',#5911);
#1673=VERTEX_POINT('',#5914);
#1674=VERTEX_POINT('',#5918);
#1675=VERTEX_POINT('',#5921);
#1676=VERTEX_POINT('',#5923);
#1677=VERTEX_POINT('',#5934);
#1678=VERTEX_POINT('',#5935);
#1679=VERTEX_POINT('',#5937);
#1680=VERTEX_POINT('',#5939);
#1681=VERTEX_POINT('',#5943);
#1682=VERTEX_POINT('',#5945);
#1683=VERTEX_POINT('',#5949);
#1684=VERTEX_POINT('',#5951);
#1685=VERTEX_POINT('',#5957);
#1686=VERTEX_POINT('',#5959);
#1687=VERTEX_POINT('',#5961);
#1688=VERTEX_POINT('',#5963);
#1689=VERTEX_POINT('',#5967);
#1690=VERTEX_POINT('',#5968);
#1691=VERTEX_POINT('',#5970);
#1692=VERTEX_POINT('',#5972);
#1693=VERTEX_POINT('',#5976);
#1694=VERTEX_POINT('',#5978);
#1695=VERTEX_POINT('',#5982);
#1696=VERTEX_POINT('',#5984);
#1697=VERTEX_POINT('',#5988);
#1698=VERTEX_POINT('',#5990);
#1699=VERTEX_POINT('',#5992);
#1700=VERTEX_POINT('',#5994);
#1701=VERTEX_POINT('',#5996);
#1702=VERTEX_POINT('',#5998);
#1703=VERTEX_POINT('',#6003);
#1704=VERTEX_POINT('',#6006);
#1705=VERTEX_POINT('',#6009);
#1706=VERTEX_POINT('',#6011);
#1707=VERTEX_POINT('',#6013);
#1708=VERTEX_POINT('',#6015);
#1709=VERTEX_POINT('',#6019);
#1710=VERTEX_POINT('',#6020);
#1711=VERTEX_POINT('',#6025);
#1712=VERTEX_POINT('',#6026);
#1713=VERTEX_POINT('',#6028);
#1714=VERTEX_POINT('',#6030);
#1715=VERTEX_POINT('',#6041);
#1716=VERTEX_POINT('',#6045);
#1717=VERTEX_POINT('',#6047);
#1718=VERTEX_POINT('',#6055);
#1719=VERTEX_POINT('',#6852);
#1720=VERTEX_POINT('',#6854);
#1721=VERTEX_POINT('',#6939);
#1722=VERTEX_POINT('',#6940);
#1723=VERTEX_POINT('',#6942);
#1724=VERTEX_POINT('',#6944);
#1725=VERTEX_POINT('',#6948);
#1726=VERTEX_POINT('',#6950);
#1727=VERTEX_POINT('',#6954);
#1728=VERTEX_POINT('',#6956);
#1729=VERTEX_POINT('',#6963);
#1730=VERTEX_POINT('',#6964);
#1731=VERTEX_POINT('',#6966);
#1732=VERTEX_POINT('',#6968);
#1733=VERTEX_POINT('',#6972);
#1734=VERTEX_POINT('',#6974);
#1735=VERTEX_POINT('',#6978);
#1736=VERTEX_POINT('',#6982);
#1737=VERTEX_POINT('',#6983);
#1738=VERTEX_POINT('',#6985);
#1739=VERTEX_POINT('',#6987);
#1740=VERTEX_POINT('',#6991);
#1741=VERTEX_POINT('',#6993);
#1742=VERTEX_POINT('',#6997);
#1743=VERTEX_POINT('',#6999);
#1744=VERTEX_POINT('',#7007);
#1745=EDGE_CURVE('',#1432,#1433,#1415,.T.);
#1746=EDGE_CURVE('',#1434,#1432,#827,.T.);
#1747=EDGE_CURVE('',#1434,#1435,#795,.F.);
#1748=EDGE_CURVE('',#1435,#1436,#662,.F.);
#1749=EDGE_CURVE('',#1437,#1436,#796,.T.);
#1750=EDGE_CURVE('',#1433,#1437,#828,.T.);
#1751=EDGE_CURVE('',#1433,#1438,#663,.T.);
#1752=EDGE_CURVE('',#1438,#1437,#829,.F.);
#1753=EDGE_CURVE('',#1438,#1439,#664,.T.);
#1754=EDGE_CURVE('',#1436,#1440,#830,.F.);
#1755=EDGE_CURVE('',#1441,#1440,#797,.F.);
#1756=EDGE_CURVE('',#1439,#1441,#831,.T.);
#1757=EDGE_CURVE('',#1439,#1442,#665,.T.);
#1758=EDGE_CURVE('',#1441,#1442,#832,.T.);
#1759=EDGE_CURVE('',#1442,#1443,#1416,.T.);
#1760=EDGE_CURVE('',#1440,#1444,#666,.F.);
#1761=EDGE_CURVE('',#1445,#1444,#798,.T.);
#1762=EDGE_CURVE('',#1443,#1445,#833,.T.);
#1763=EDGE_CURVE('',#1443,#1446,#667,.T.);
#1764=EDGE_CURVE('',#1446,#1445,#834,.F.);
#1765=EDGE_CURVE('',#1446,#1447,#668,.T.);
#1766=EDGE_CURVE('',#1444,#1448,#835,.F.);
#1767=EDGE_CURVE('',#1449,#1448,#799,.F.);
#1768=EDGE_CURVE('',#1447,#1449,#836,.T.);
#1769=EDGE_CURVE('',#1447,#1450,#669,.T.);
#1770=EDGE_CURVE('',#1449,#1450,#837,.T.);
#1771=EDGE_CURVE('',#1451,#1452,#1417,.T.);
#1772=EDGE_CURVE('',#1453,#1451,#838,.T.);
#1773=EDGE_CURVE('',#1453,#1454,#800,.F.);
#1774=EDGE_CURVE('',#1454,#1455,#670,.F.);
#1775=EDGE_CURVE('',#1456,#1455,#801,.T.);
#1776=EDGE_CURVE('',#1452,#1456,#839,.T.);
#1777=EDGE_CURVE('',#1452,#1457,#671,.T.);
#1778=EDGE_CURVE('',#1457,#1456,#840,.F.);
#1779=EDGE_CURVE('',#1450,#1458,#1418,.T.);
#1780=EDGE_CURVE('',#1448,#1459,#672,.F.);
#1781=EDGE_CURVE('',#1460,#1459,#802,.T.);
#1782=EDGE_CURVE('',#1458,#1460,#841,.T.);
#1783=EDGE_CURVE('',#1458,#1461,#673,.T.);
#1784=EDGE_CURVE('',#1461,#1460,#842,.F.);
#1785=EDGE_CURVE('',#1462,#1432,#674,.T.);
#1786=EDGE_CURVE('',#1462,#1434,#843,.T.);
#1787=EDGE_CURVE('',#1457,#1463,#675,.T.);
#1788=EDGE_CURVE('',#1455,#1435,#844,.F.);
#1789=EDGE_CURVE('',#1463,#1462,#676,.T.);
#1790=EDGE_CURVE('',#1464,#1451,#677,.T.);
#1791=EDGE_CURVE('',#1464,#1453,#845,.T.);
#1792=EDGE_CURVE('',#1461,#1464,#678,.T.);
#1793=EDGE_CURVE('',#1459,#1454,#846,.F.);
#1794=EDGE_CURVE('',#1465,#1465,#679,.T.);
#1795=EDGE_CURVE('',#1465,#1466,#680,.T.);
#1796=EDGE_CURVE('',#1466,#1466,#681,.T.);
#1797=EDGE_CURVE('',#1467,#1467,#682,.T.);
#1798=EDGE_CURVE('',#1468,#1468,#683,.T.);
#1799=EDGE_CURVE('',#1468,#1466,#847,.T.);
#1800=EDGE_CURVE('',#1469,#1469,#684,.T.);
#1801=EDGE_CURVE('',#1469,#1468,#848,.T.);
#1802=EDGE_CURVE('',#1470,#1470,#685,.F.);
#1803=EDGE_CURVE('',#1470,#1469,#849,.T.);
#1804=EDGE_CURVE('',#1463,#1471,#686,.T.);
#1805=EDGE_CURVE('',#1472,#1471,#687,.T.);
#1806=EDGE_CURVE('',#1471,#1472,#688,.T.);
#1807=EDGE_CURVE('',#1467,#1472,#850,.T.);
#1808=EDGE_CURVE('',#1473,#1474,#1419,.T.);
#1809=EDGE_CURVE('',#1475,#1473,#851,.T.);
#1810=EDGE_CURVE('',#1475,#1476,#803,.F.);
#1811=EDGE_CURVE('',#1476,#1477,#689,.F.);
#1812=EDGE_CURVE('',#1478,#1477,#804,.T.);
#1813=EDGE_CURVE('',#1474,#1478,#852,.T.);
#1814=EDGE_CURVE('',#1474,#1479,#690,.T.);
#1815=EDGE_CURVE('',#1479,#1478,#853,.F.);
#1816=EDGE_CURVE('',#1479,#1480,#691,.T.);
#1817=EDGE_CURVE('',#1477,#1481,#854,.F.);
#1818=EDGE_CURVE('',#1482,#1481,#805,.F.);
#1819=EDGE_CURVE('',#1480,#1482,#855,.T.);
#1820=EDGE_CURVE('',#1480,#1483,#692,.T.);
#1821=EDGE_CURVE('',#1482,#1483,#856,.T.);
#1822=EDGE_CURVE('',#1483,#1484,#1420,.T.);
#1823=EDGE_CURVE('',#1481,#1485,#693,.F.);
#1824=EDGE_CURVE('',#1486,#1485,#806,.T.);
#1825=EDGE_CURVE('',#1484,#1486,#857,.T.);
#1826=EDGE_CURVE('',#1484,#1487,#694,.T.);
#1827=EDGE_CURVE('',#1487,#1486,#858,.F.);
#1828=EDGE_CURVE('',#1487,#1488,#695,.T.);
#1829=EDGE_CURVE('',#1485,#1489,#859,.F.);
#1830=EDGE_CURVE('',#1490,#1489,#807,.F.);
#1831=EDGE_CURVE('',#1488,#1490,#860,.T.);
#1832=EDGE_CURVE('',#1488,#1491,#696,.T.);
#1833=EDGE_CURVE('',#1490,#1491,#861,.T.);
#1834=EDGE_CURVE('',#1492,#1493,#1421,.T.);
#1835=EDGE_CURVE('',#1494,#1492,#862,.T.);
#1836=EDGE_CURVE('',#1494,#1495,#808,.F.);
#1837=EDGE_CURVE('',#1495,#1496,#697,.F.);
#1838=EDGE_CURVE('',#1497,#1496,#809,.T.);
#1839=EDGE_CURVE('',#1493,#1497,#863,.T.);
#1840=EDGE_CURVE('',#1493,#1498,#698,.T.);
#1841=EDGE_CURVE('',#1498,#1497,#864,.F.);
#1842=EDGE_CURVE('',#1491,#1499,#1422,.T.);
#1843=EDGE_CURVE('',#1489,#1500,#699,.F.);
#1844=EDGE_CURVE('',#1501,#1500,#810,.T.);
#1845=EDGE_CURVE('',#1499,#1501,#865,.T.);
#1846=EDGE_CURVE('',#1499,#1502,#700,.T.);
#1847=EDGE_CURVE('',#1502,#1501,#866,.F.);
#1848=EDGE_CURVE('',#1503,#1473,#701,.T.);
#1849=EDGE_CURVE('',#1503,#1475,#867,.T.);
#1850=EDGE_CURVE('',#1498,#1504,#702,.T.);
#1851=EDGE_CURVE('',#1496,#1476,#868,.F.);
#1852=EDGE_CURVE('',#1504,#1503,#703,.T.);
#1853=EDGE_CURVE('',#1505,#1492,#704,.T.);
#1854=EDGE_CURVE('',#1505,#1494,#869,.T.);
#1855=EDGE_CURVE('',#1502,#1505,#705,.T.);
#1856=EDGE_CURVE('',#1500,#1495,#870,.F.);
#1857=EDGE_CURVE('',#1506,#1506,#706,.T.);
#1858=EDGE_CURVE('',#1506,#1507,#707,.T.);
#1859=EDGE_CURVE('',#1507,#1507,#708,.T.);
#1860=EDGE_CURVE('',#1508,#1508,#709,.T.);
#1861=EDGE_CURVE('',#1509,#1509,#710,.T.);
#1862=EDGE_CURVE('',#1509,#1507,#871,.T.);
#1863=EDGE_CURVE('',#1510,#1510,#711,.T.);
#1864=EDGE_CURVE('',#1510,#1509,#872,.T.);
#1865=EDGE_CURVE('',#1511,#1511,#712,.F.);
#1866=EDGE_CURVE('',#1511,#1510,#873,.T.);
#1867=EDGE_CURVE('',#1504,#1512,#713,.T.);
#1868=EDGE_CURVE('',#1513,#1512,#714,.T.);
#1869=EDGE_CURVE('',#1512,#1513,#715,.T.);
#1870=EDGE_CURVE('',#1508,#1513,#874,.T.);
#1871=EDGE_CURVE('',#1514,#1515,#1423,.T.);
#1872=EDGE_CURVE('',#1516,#1514,#875,.T.);
#1873=EDGE_CURVE('',#1516,#1517,#811,.F.);
#1874=EDGE_CURVE('',#1517,#1518,#716,.F.);
#1875=EDGE_CURVE('',#1519,#1518,#812,.T.);
#1876=EDGE_CURVE('',#1515,#1519,#876,.T.);
#1877=EDGE_CURVE('',#1515,#1520,#717,.T.);
#1878=EDGE_CURVE('',#1520,#1519,#877,.F.);
#1879=EDGE_CURVE('',#1520,#1521,#718,.T.);
#1880=EDGE_CURVE('',#1518,#1522,#878,.F.);
#1881=EDGE_CURVE('',#1523,#1522,#813,.F.);
#1882=EDGE_CURVE('',#1521,#1523,#879,.T.);
#1883=EDGE_CURVE('',#1521,#1524,#719,.T.);
#1884=EDGE_CURVE('',#1523,#1524,#880,.T.);
#1885=EDGE_CURVE('',#1524,#1525,#1424,.T.);
#1886=EDGE_CURVE('',#1522,#1526,#720,.F.);
#1887=EDGE_CURVE('',#1527,#1526,#814,.T.);
#1888=EDGE_CURVE('',#1525,#1527,#881,.T.);
#1889=EDGE_CURVE('',#1525,#1528,#721,.T.);
#1890=EDGE_CURVE('',#1528,#1527,#882,.F.);
#1891=EDGE_CURVE('',#1528,#1529,#722,.T.);
#1892=EDGE_CURVE('',#1526,#1530,#883,.F.);
#1893=EDGE_CURVE('',#1531,#1530,#815,.F.);
#1894=EDGE_CURVE('',#1529,#1531,#884,.T.);
#1895=EDGE_CURVE('',#1529,#1532,#723,.T.);
#1896=EDGE_CURVE('',#1531,#1532,#885,.T.);
#1897=EDGE_CURVE('',#1533,#1534,#1425,.T.);
#1898=EDGE_CURVE('',#1535,#1533,#886,.T.);
#1899=EDGE_CURVE('',#1535,#1536,#816,.F.);
#1900=EDGE_CURVE('',#1536,#1537,#724,.F.);
#1901=EDGE_CURVE('',#1538,#1537,#817,.T.);
#1902=EDGE_CURVE('',#1534,#1538,#887,.T.);
#1903=EDGE_CURVE('',#1534,#1539,#725,.T.);
#1904=EDGE_CURVE('',#1539,#1538,#888,.F.);
#1905=EDGE_CURVE('',#1532,#1540,#1426,.T.);
#1906=EDGE_CURVE('',#1530,#1541,#726,.F.);
#1907=EDGE_CURVE('',#1542,#1541,#818,.T.);
#1908=EDGE_CURVE('',#1540,#1542,#889,.T.);
#1909=EDGE_CURVE('',#1540,#1543,#727,.T.);
#1910=EDGE_CURVE('',#1543,#1542,#890,.F.);
#1911=EDGE_CURVE('',#1544,#1514,#728,.T.);
#1912=EDGE_CURVE('',#1544,#1516,#891,.T.);
#1913=EDGE_CURVE('',#1539,#1545,#729,.T.);
#1914=EDGE_CURVE('',#1537,#1517,#892,.F.);
#1915=EDGE_CURVE('',#1545,#1544,#730,.T.);
#1916=EDGE_CURVE('',#1546,#1533,#731,.T.);
#1917=EDGE_CURVE('',#1546,#1535,#893,.T.);
#1918=EDGE_CURVE('',#1543,#1546,#732,.T.);
#1919=EDGE_CURVE('',#1541,#1536,#894,.F.);
#1920=EDGE_CURVE('',#1547,#1547,#733,.T.);
#1921=EDGE_CURVE('',#1547,#1548,#734,.T.);
#1922=EDGE_CURVE('',#1548,#1548,#735,.T.);
#1923=EDGE_CURVE('',#1549,#1549,#736,.T.);
#1924=EDGE_CURVE('',#1550,#1550,#737,.T.);
#1925=EDGE_CURVE('',#1550,#1548,#895,.T.);
#1926=EDGE_CURVE('',#1551,#1551,#738,.T.);
#1927=EDGE_CURVE('',#1551,#1550,#896,.T.);
#1928=EDGE_CURVE('',#1552,#1552,#739,.F.);
#1929=EDGE_CURVE('',#1552,#1551,#897,.T.);
#1930=EDGE_CURVE('',#1545,#1553,#740,.T.);
#1931=EDGE_CURVE('',#1554,#1553,#741,.T.);
#1932=EDGE_CURVE('',#1553,#1554,#742,.T.);
#1933=EDGE_CURVE('',#1549,#1554,#898,.T.);
#1934=EDGE_CURVE('',#1555,#1556,#1427,.T.);
#1935=EDGE_CURVE('',#1557,#1555,#899,.T.);
#1936=EDGE_CURVE('',#1557,#1558,#819,.F.);
#1937=EDGE_CURVE('',#1558,#1559,#743,.F.);
#1938=EDGE_CURVE('',#1560,#1559,#820,.T.);
#1939=EDGE_CURVE('',#1556,#1560,#900,.T.);
#1940=EDGE_CURVE('',#1556,#1561,#744,.T.);
#1941=EDGE_CURVE('',#1561,#1560,#901,.F.);
#1942=EDGE_CURVE('',#1561,#1562,#745,.T.);
#1943=EDGE_CURVE('',#1559,#1563,#902,.F.);
#1944=EDGE_CURVE('',#1564,#1563,#821,.F.);
#1945=EDGE_CURVE('',#1562,#1564,#903,.T.);
#1946=EDGE_CURVE('',#1562,#1565,#746,.T.);
#1947=EDGE_CURVE('',#1564,#1565,#904,.T.);
#1948=EDGE_CURVE('',#1565,#1566,#1428,.T.);
#1949=EDGE_CURVE('',#1563,#1567,#747,.F.);
#1950=EDGE_CURVE('',#1568,#1567,#822,.T.);
#1951=EDGE_CURVE('',#1566,#1568,#905,.T.);
#1952=EDGE_CURVE('',#1566,#1569,#748,.T.);
#1953=EDGE_CURVE('',#1569,#1568,#906,.F.);
#1954=EDGE_CURVE('',#1569,#1570,#749,.T.);
#1955=EDGE_CURVE('',#1567,#1571,#907,.F.);
#1956=EDGE_CURVE('',#1572,#1571,#823,.F.);
#1957=EDGE_CURVE('',#1570,#1572,#908,.T.);
#1958=EDGE_CURVE('',#1570,#1573,#750,.T.);
#1959=EDGE_CURVE('',#1572,#1573,#909,.T.);
#1960=EDGE_CURVE('',#1574,#1575,#1429,.T.);
#1961=EDGE_CURVE('',#1576,#1574,#910,.T.);
#1962=EDGE_CURVE('',#1576,#1577,#824,.F.);
#1963=EDGE_CURVE('',#1577,#1578,#751,.F.);
#1964=EDGE_CURVE('',#1579,#1578,#825,.T.);
#1965=EDGE_CURVE('',#1575,#1579,#911,.T.);
#1966=EDGE_CURVE('',#1575,#1580,#752,.T.);
#1967=EDGE_CURVE('',#1580,#1579,#912,.F.);
#1968=EDGE_CURVE('',#1573,#1581,#1430,.T.);
#1969=EDGE_CURVE('',#1571,#1582,#753,.F.);
#1970=EDGE_CURVE('',#1583,#1582,#826,.T.);
#1971=EDGE_CURVE('',#1581,#1583,#913,.T.);
#1972=EDGE_CURVE('',#1581,#1584,#754,.T.);
#1973=EDGE_CURVE('',#1584,#1583,#914,.F.);
#1974=EDGE_CURVE('',#1585,#1555,#755,.T.);
#1975=EDGE_CURVE('',#1585,#1557,#915,.T.);
#1976=EDGE_CURVE('',#1580,#1586,#756,.T.);
#1977=EDGE_CURVE('',#1578,#1558,#916,.F.);
#1978=EDGE_CURVE('',#1586,#1585,#757,.T.);
#1979=EDGE_CURVE('',#1587,#1574,#758,.T.);
#1980=EDGE_CURVE('',#1587,#1576,#917,.T.);
#1981=EDGE_CURVE('',#1584,#1587,#759,.T.);
#1982=EDGE_CURVE('',#1582,#1577,#918,.F.);
#1983=EDGE_CURVE('',#1588,#1588,#760,.T.);
#1984=EDGE_CURVE('',#1588,#1589,#761,.T.);
#1985=EDGE_CURVE('',#1589,#1589,#762,.T.);
#1986=EDGE_CURVE('',#1590,#1590,#763,.T.);
#1987=EDGE_CURVE('',#1591,#1591,#764,.T.);
#1988=EDGE_CURVE('',#1591,#1589,#919,.T.);
#1989=EDGE_CURVE('',#1592,#1592,#765,.T.);
#1990=EDGE_CURVE('',#1592,#1591,#920,.T.);
#1991=EDGE_CURVE('',#1593,#1593,#766,.F.);
#1992=EDGE_CURVE('',#1593,#1592,#921,.T.);
#1993=EDGE_CURVE('',#1586,#1594,#767,.T.);
#1994=EDGE_CURVE('',#1595,#1594,#768,.T.);
#1995=EDGE_CURVE('',#1594,#1595,#769,.T.);
#1996=EDGE_CURVE('',#1590,#1595,#922,.T.);
#1997=EDGE_CURVE('',#1596,#1597,#923,.T.);
#1998=EDGE_CURVE('',#1598,#1596,#924,.T.);
#1999=EDGE_CURVE('',#1599,#1598,#925,.T.);
#2000=EDGE_CURVE('',#1597,#1599,#926,.T.);
#2001=EDGE_CURVE('',#1597,#1600,#927,.T.);
#2002=EDGE_CURVE('',#1601,#1599,#928,.T.);
#2003=EDGE_CURVE('',#1600,#1601,#929,.T.);
#2004=EDGE_CURVE('',#1600,#1602,#930,.T.);
#2005=EDGE_CURVE('',#1603,#1601,#931,.T.);
#2006=EDGE_CURVE('',#1602,#1603,#932,.T.);
#2007=EDGE_CURVE('',#1603,#1598,#933,.T.);
#2008=EDGE_CURVE('',#1596,#1604,#934,.T.);
#2009=EDGE_CURVE('',#1604,#1605,#935,.T.);
#2010=EDGE_CURVE('',#1605,#1606,#936,.T.);
#2011=EDGE_CURVE('',#1606,#1607,#937,.T.);
#2012=EDGE_CURVE('',#1607,#1602,#938,.T.);
#2013=EDGE_CURVE('',#1608,#1608,#770,.F.);
#2014=EDGE_CURVE('',#1609,#1609,#771,.F.);
#2015=EDGE_CURVE('',#1610,#1607,#939,.T.);
#2016=EDGE_CURVE('',#1611,#1610,#940,.T.);
#2017=EDGE_CURVE('',#1604,#1611,#941,.T.);
#2018=EDGE_CURVE('',#1610,#1612,#942,.T.);
#2019=EDGE_CURVE('',#1612,#1613,#943,.T.);
#2020=EDGE_CURVE('',#1613,#1611,#944,.T.);
#2021=EDGE_CURVE('',#1614,#1614,#772,.T.);
#2022=EDGE_CURVE('',#1615,#1615,#773,.T.);
#2023=EDGE_CURVE('',#1606,#1612,#945,.T.);
#2024=EDGE_CURVE('',#1605,#1613,#946,.T.);
#2025=EDGE_CURVE('',#1615,#1608,#947,.T.);
#2026=EDGE_CURVE('',#1614,#1609,#948,.T.);
#2027=EDGE_CURVE('',#1616,#1617,#949,.T.);
#2028=EDGE_CURVE('',#1616,#1618,#950,.T.);
#2029=EDGE_CURVE('',#1619,#1618,#951,.T.);
#2030=EDGE_CURVE('',#1617,#1619,#952,.T.);
#2031=EDGE_CURVE('',#1617,#1620,#953,.T.);
#2032=EDGE_CURVE('',#1621,#1619,#954,.T.);
#2033=EDGE_CURVE('',#1620,#1621,#955,.T.);
#2034=EDGE_CURVE('',#1620,#1622,#956,.T.);
#2035=EDGE_CURVE('',#1623,#1621,#957,.T.);
#2036=EDGE_CURVE('',#1622,#1623,#958,.T.);
#2037=EDGE_CURVE('',#1618,#1623,#959,.T.);
#2038=EDGE_CURVE('',#1624,#1622,#960,.T.);
#2039=EDGE_CURVE('',#1625,#1624,#961,.T.);
#2040=EDGE_CURVE('',#1626,#1625,#962,.T.);
#2041=EDGE_CURVE('',#1627,#1626,#963,.T.);
#2042=EDGE_CURVE('',#1616,#1627,#964,.T.);
#2043=EDGE_CURVE('',#1628,#1628,#774,.T.);
#2044=EDGE_CURVE('',#1628,#1629,#965,.T.);
#2045=EDGE_CURVE('',#1629,#1629,#775,.T.);
#2046=EDGE_CURVE('',#1630,#1631,#966,.T.);
#2047=EDGE_CURVE('',#1632,#1630,#967,.T.);
#2048=EDGE_CURVE('',#1633,#1632,#968,.T.);
#2049=EDGE_CURVE('',#1631,#1633,#969,.T.);
#2050=EDGE_CURVE('',#1634,#1635,#970,.T.);
#2051=EDGE_CURVE('',#1636,#1634,#971,.T.);
#2052=EDGE_CURVE('',#1637,#1636,#972,.T.);
#2053=EDGE_CURVE('',#1637,#1635,#973,.T.);
#2054=EDGE_CURVE('',#1635,#1630,#974,.T.);
#2055=EDGE_CURVE('',#1632,#1637,#975,.T.);
#2056=EDGE_CURVE('',#1638,#1633,#976,.T.);
#2057=EDGE_CURVE('',#1638,#1639,#977,.T.);
#2058=EDGE_CURVE('',#1639,#1640,#978,.T.);
#2059=EDGE_CURVE('',#1640,#1641,#979,.T.);
#2060=EDGE_CURVE('',#1631,#1641,#980,.T.);
#2061=EDGE_CURVE('',#1642,#1643,#981,.T.);
#2062=EDGE_CURVE('',#1642,#1644,#982,.T.);
#2063=EDGE_CURVE('',#1645,#1644,#983,.T.);
#2064=EDGE_CURVE('',#1643,#1645,#984,.T.);
#2065=EDGE_CURVE('',#1646,#1638,#985,.T.);
#2066=EDGE_CURVE('',#1646,#1647,#986,.T.);
#2067=EDGE_CURVE('',#1647,#1639,#987,.T.);
#2068=EDGE_CURVE('',#1645,#1646,#988,.T.);
#2069=EDGE_CURVE('',#1644,#1647,#989,.T.);
#2070=EDGE_CURVE('',#1640,#1642,#776,.T.);
#2071=EDGE_CURVE('',#1648,#1649,#990,.T.);
#2072=EDGE_CURVE('',#1648,#1650,#991,.T.);
#2073=EDGE_CURVE('',#1651,#1650,#992,.T.);
#2074=EDGE_CURVE('',#1649,#1651,#993,.T.);
#2075=EDGE_CURVE('',#1650,#1634,#777,.T.);
#2076=EDGE_CURVE('',#1636,#1648,#778,.T.);
#2077=EDGE_CURVE('',#1652,#1653,#994,.T.);
#2078=EDGE_CURVE('',#1627,#1653,#995,.T.);
#2079=EDGE_CURVE('',#1652,#1626,#996,.T.);
#2080=EDGE_CURVE('',#1654,#1655,#997,.T.);
#2081=EDGE_CURVE('',#1655,#1624,#998,.T.);
#2082=EDGE_CURVE('',#1653,#1651,#999,.T.);
#2083=EDGE_CURVE('',#1641,#1654,#779,.T.);
#2084=EDGE_CURVE('',#1649,#1652,#1000,.T.);
#2085=EDGE_CURVE('',#1656,#1643,#1001,.T.);
#2086=EDGE_CURVE('',#1625,#1656,#1002,.T.);
#2087=EDGE_CURVE('',#1642,#1654,#1003,.T.);
#2088=EDGE_CURVE('',#1655,#1656,#1004,.T.);
#2089=EDGE_CURVE('',#1657,#1658,#1005,.T.);
#2090=EDGE_CURVE('',#1659,#1657,#1006,.T.);
#2091=EDGE_CURVE('',#1659,#1660,#1007,.T.);
#2092=EDGE_CURVE('',#1658,#1660,#1008,.T.);
#2093=EDGE_CURVE('',#1658,#1661,#1009,.T.);
#2094=EDGE_CURVE('',#1660,#1662,#1010,.T.);
#2095=EDGE_CURVE('',#1661,#1662,#1011,.T.);
#2096=EDGE_CURVE('',#1661,#1663,#1012,.T.);
#2097=EDGE_CURVE('',#1662,#1664,#1013,.T.);
#2098=EDGE_CURVE('',#1663,#1664,#1014,.T.);
#2099=EDGE_CURVE('',#1664,#1659,#1015,.T.);
#2100=EDGE_CURVE('',#1665,#1663,#1016,.T.);
#2101=EDGE_CURVE('',#1666,#1665,#1017,.T.);
#2102=EDGE_CURVE('',#1667,#1666,#1018,.T.);
#2103=EDGE_CURVE('',#1668,#1667,#1019,.T.);
#2104=EDGE_CURVE('',#1657,#1668,#1020,.T.);
#2105=EDGE_CURVE('',#1666,#1669,#1021,.T.);
#2106=EDGE_CURVE('',#1669,#1670,#1022,.T.);
#2107=EDGE_CURVE('',#1670,#1667,#1023,.T.);
#2108=EDGE_CURVE('',#1671,#1671,#780,.T.);
#2109=EDGE_CURVE('',#1672,#1672,#781,.T.);
#2110=EDGE_CURVE('',#1673,#1670,#1024,.T.);
#2111=EDGE_CURVE('',#1668,#1673,#1025,.T.);
#2112=EDGE_CURVE('',#1673,#1674,#1026,.T.);
#2113=EDGE_CURVE('',#1674,#1665,#1027,.T.);
#2114=EDGE_CURVE('',#1675,#1675,#782,.F.);
#2115=EDGE_CURVE('',#1676,#1676,#783,.F.);
#2116=EDGE_CURVE('',#1674,#1669,#1028,.T.);
#2117=EDGE_CURVE('',#1672,#1676,#1029,.T.);
#2118=EDGE_CURVE('',#1671,#1675,#1030,.T.);
#2119=EDGE_CURVE('',#1677,#1678,#1031,.T.);
#2120=EDGE_CURVE('',#1677,#1679,#1032,.T.);
#2121=EDGE_CURVE('',#1679,#1680,#1033,.T.);
#2122=EDGE_CURVE('',#1678,#1680,#1034,.T.);
#2123=EDGE_CURVE('',#1681,#1677,#1035,.T.);
#2124=EDGE_CURVE('',#1681,#1682,#1036,.T.);
#2125=EDGE_CURVE('',#1682,#1679,#1037,.T.);
#2126=EDGE_CURVE('',#1683,#1681,#1038,.T.);
#2127=EDGE_CURVE('',#1683,#1684,#1039,.T.);
#2128=EDGE_CURVE('',#1684,#1682,#1040,.T.);
#2129=EDGE_CURVE('',#1680,#1684,#1041,.T.);
#2130=EDGE_CURVE('',#1685,#1678,#1042,.T.);
#2131=EDGE_CURVE('',#1685,#1686,#1043,.T.);
#2132=EDGE_CURVE('',#1687,#1686,#1044,.T.);
#2133=EDGE_CURVE('',#1688,#1687,#1045,.T.);
#2134=EDGE_CURVE('',#1683,#1688,#1046,.T.);
#2135=EDGE_CURVE('',#1689,#1690,#1047,.T.);
#2136=EDGE_CURVE('',#1691,#1689,#1048,.T.);
#2137=EDGE_CURVE('',#1692,#1691,#1049,.T.);
#2138=EDGE_CURVE('',#1690,#1692,#1050,.T.);
#2139=EDGE_CURVE('',#1693,#1685,#1051,.T.);
#2140=EDGE_CURVE('',#1694,#1693,#1052,.T.);
#2141=EDGE_CURVE('',#1686,#1694,#1053,.T.);
#2142=EDGE_CURVE('',#1695,#1692,#784,.T.);
#2143=EDGE_CURVE('',#1695,#1696,#1054,.T.);
#2144=EDGE_CURVE('',#1690,#1696,#785,.T.);
#2145=EDGE_CURVE('',#1696,#1697,#1055,.T.);
#2146=EDGE_CURVE('',#1697,#1698,#786,.T.);
#2147=EDGE_CURVE('',#1698,#1699,#1056,.T.);
#2148=EDGE_CURVE('',#1699,#1700,#1057,.T.);
#2149=EDGE_CURVE('',#1700,#1701,#1058,.T.);
#2150=EDGE_CURVE('',#1701,#1702,#1059,.T.);
#2151=EDGE_CURVE('',#1702,#1693,#787,.T.);
#2152=EDGE_CURVE('',#1688,#1689,#1060,.T.);
#2153=EDGE_CURVE('',#1703,#1695,#1061,.T.);
#2154=EDGE_CURVE('',#1703,#1697,#1062,.T.);
#2155=EDGE_CURVE('',#1704,#1704,#788,.T.);
#2156=EDGE_CURVE('',#1705,#1699,#1063,.T.);
#2157=EDGE_CURVE('',#1706,#1698,#1064,.T.);
#2158=EDGE_CURVE('',#1706,#1707,#1065,.T.);
#2159=EDGE_CURVE('',#1707,#1708,#1066,.T.);
#2160=EDGE_CURVE('',#1705,#1708,#1067,.T.);
#2161=EDGE_CURVE('',#1709,#1710,#1068,.T.);
#2162=EDGE_CURVE('',#1710,#1706,#789,.T.);
#2163=EDGE_CURVE('',#1709,#1703,#790,.T.);
#2164=EDGE_CURVE('',#1711,#1712,#1069,.T.);
#2165=EDGE_CURVE('',#1711,#1713,#1070,.T.);
#2166=EDGE_CURVE('',#1713,#1714,#1071,.T.);
#2167=EDGE_CURVE('',#1712,#1714,#1072,.T.);
#2168=EDGE_CURVE('',#1707,#1713,#1073,.T.);
#2169=EDGE_CURVE('',#1708,#1711,#1074,.T.);
#2170=EDGE_CURVE('',#1714,#1710,#1075,.T.);
#2171=EDGE_CURVE('',#1712,#1709,#1076,.T.);
#2172=EDGE_CURVE('',#1702,#1715,#1077,.T.);
#2173=EDGE_CURVE('',#1694,#1715,#791,.T.);
#2174=EDGE_CURVE('',#1716,#1700,#1078,.T.);
#2175=EDGE_CURVE('',#1717,#1716,#1079,.T.);
#2176=EDGE_CURVE('',#1717,#1701,#1080,.T.);
#2177=EDGE_CURVE('',#1716,#1705,#1081,.T.);
#2178=EDGE_CURVE('',#1715,#1717,#1082,.T.);
#2179=EDGE_CURVE('',#1718,#1718,#792,.T.);
#2180=EDGE_CURVE('',#1718,#1704,#1083,.T.);
#2181=EDGE_CURVE('',#1691,#1687,#1084,.T.);
#2182=EDGE_CURVE('',#1719,#1719,#793,.T.);
#2183=EDGE_CURVE('',#1719,#1720,#1431,.T.);
#2184=EDGE_CURVE('',#1720,#1720,#794,.T.);
#2185=EDGE_CURVE('',#1721,#1722,#1085,.T.);
#2186=EDGE_CURVE('',#1721,#1723,#1086,.T.);
#2187=EDGE_CURVE('',#1723,#1724,#1087,.T.);
#2188=EDGE_CURVE('',#1722,#1724,#1088,.T.);
#2189=EDGE_CURVE('',#1725,#1721,#1089,.T.);
#2190=EDGE_CURVE('',#1725,#1726,#1090,.T.);
#2191=EDGE_CURVE('',#1726,#1723,#1091,.T.);
#2192=EDGE_CURVE('',#1727,#1725,#1092,.T.);
#2193=EDGE_CURVE('',#1727,#1728,#1093,.T.);
#2194=EDGE_CURVE('',#1728,#1726,#1094,.T.);
#2195=EDGE_CURVE('',#1722,#1727,#1095,.T.);
#2196=EDGE_CURVE('',#1724,#1728,#1096,.T.);
#2197=EDGE_CURVE('',#1729,#1730,#1097,.T.);
#2198=EDGE_CURVE('',#1731,#1729,#1098,.T.);
#2199=EDGE_CURVE('',#1732,#1731,#1099,.T.);
#2200=EDGE_CURVE('',#1730,#1732,#1100,.T.);
#2201=EDGE_CURVE('',#1729,#1733,#1101,.T.);
#2202=EDGE_CURVE('',#1734,#1733,#1102,.T.);
#2203=EDGE_CURVE('',#1731,#1734,#1103,.T.);
#2204=EDGE_CURVE('',#1730,#1735,#1104,.T.);
#2205=EDGE_CURVE('',#1733,#1735,#1105,.T.);
#2206=EDGE_CURVE('',#1736,#1737,#1106,.T.);
#2207=EDGE_CURVE('',#1736,#1738,#1107,.T.);
#2208=EDGE_CURVE('',#1738,#1739,#1108,.T.);
#2209=EDGE_CURVE('',#1737,#1739,#1109,.T.);
#2210=EDGE_CURVE('',#1740,#1736,#1110,.T.);
#2211=EDGE_CURVE('',#1740,#1741,#1111,.T.);
#2212=EDGE_CURVE('',#1741,#1738,#1112,.T.);
#2213=EDGE_CURVE('',#1742,#1740,#1113,.T.);
#2214=EDGE_CURVE('',#1742,#1743,#1114,.T.);
#2215=EDGE_CURVE('',#1743,#1741,#1115,.T.);
#2216=EDGE_CURVE('',#1737,#1742,#1116,.T.);
#2217=EDGE_CURVE('',#1739,#1743,#1117,.T.);
#2218=EDGE_CURVE('',#1744,#1734,#1118,.T.);
#2219=EDGE_CURVE('',#1732,#1744,#1119,.T.);
#2220=EDGE_CURVE('',#1735,#1744,#1120,.T.);
#2221=ORIENTED_EDGE('',*,*,#1745,.F.);
#2222=ORIENTED_EDGE('',*,*,#1746,.F.);
#2223=ORIENTED_EDGE('',*,*,#1747,.T.);
#2224=ORIENTED_EDGE('',*,*,#1748,.T.);
#2225=ORIENTED_EDGE('',*,*,#1749,.F.);
#2226=ORIENTED_EDGE('',*,*,#1750,.F.);
#2227=ORIENTED_EDGE('',*,*,#1751,.F.);
#2228=ORIENTED_EDGE('',*,*,#1750,.T.);
#2229=ORIENTED_EDGE('',*,*,#1752,.F.);
#2230=ORIENTED_EDGE('',*,*,#1753,.F.);
#2231=ORIENTED_EDGE('',*,*,#1752,.T.);
#2232=ORIENTED_EDGE('',*,*,#1749,.T.);
#2233=ORIENTED_EDGE('',*,*,#1754,.T.);
#2234=ORIENTED_EDGE('',*,*,#1755,.F.);
#2235=ORIENTED_EDGE('',*,*,#1756,.F.);
#2236=ORIENTED_EDGE('',*,*,#1757,.F.);
#2237=ORIENTED_EDGE('',*,*,#1756,.T.);
#2238=ORIENTED_EDGE('',*,*,#1758,.T.);
#2239=ORIENTED_EDGE('',*,*,#1759,.F.);
#2240=ORIENTED_EDGE('',*,*,#1758,.F.);
#2241=ORIENTED_EDGE('',*,*,#1755,.T.);
#2242=ORIENTED_EDGE('',*,*,#1760,.T.);
#2243=ORIENTED_EDGE('',*,*,#1761,.F.);
#2244=ORIENTED_EDGE('',*,*,#1762,.F.);
#2245=ORIENTED_EDGE('',*,*,#1763,.F.);
#2246=ORIENTED_EDGE('',*,*,#1762,.T.);
#2247=ORIENTED_EDGE('',*,*,#1764,.F.);
#2248=ORIENTED_EDGE('',*,*,#1765,.F.);
#2249=ORIENTED_EDGE('',*,*,#1764,.T.);
#2250=ORIENTED_EDGE('',*,*,#1761,.T.);
#2251=ORIENTED_EDGE('',*,*,#1766,.T.);
#2252=ORIENTED_EDGE('',*,*,#1767,.F.);
#2253=ORIENTED_EDGE('',*,*,#1768,.F.);
#2254=ORIENTED_EDGE('',*,*,#1769,.F.);
#2255=ORIENTED_EDGE('',*,*,#1768,.T.);
#2256=ORIENTED_EDGE('',*,*,#1770,.T.);
#2257=ORIENTED_EDGE('',*,*,#1771,.F.);
#2258=ORIENTED_EDGE('',*,*,#1772,.F.);
#2259=ORIENTED_EDGE('',*,*,#1773,.T.);
#2260=ORIENTED_EDGE('',*,*,#1774,.T.);
#2261=ORIENTED_EDGE('',*,*,#1775,.F.);
#2262=ORIENTED_EDGE('',*,*,#1776,.F.);
#2263=ORIENTED_EDGE('',*,*,#1777,.F.);
#2264=ORIENTED_EDGE('',*,*,#1776,.T.);
#2265=ORIENTED_EDGE('',*,*,#1778,.F.);
#2266=ORIENTED_EDGE('',*,*,#1779,.F.);
#2267=ORIENTED_EDGE('',*,*,#1770,.F.);
#2268=ORIENTED_EDGE('',*,*,#1767,.T.);
#2269=ORIENTED_EDGE('',*,*,#1780,.T.);
#2270=ORIENTED_EDGE('',*,*,#1781,.F.);
#2271=ORIENTED_EDGE('',*,*,#1782,.F.);
#2272=ORIENTED_EDGE('',*,*,#1783,.F.);
#2273=ORIENTED_EDGE('',*,*,#1782,.T.);
#2274=ORIENTED_EDGE('',*,*,#1784,.F.);
#2275=ORIENTED_EDGE('',*,*,#1785,.F.);
#2276=ORIENTED_EDGE('',*,*,#1786,.T.);
#2277=ORIENTED_EDGE('',*,*,#1746,.T.);
#2278=ORIENTED_EDGE('',*,*,#1787,.F.);
#2279=ORIENTED_EDGE('',*,*,#1778,.T.);
#2280=ORIENTED_EDGE('',*,*,#1775,.T.);
#2281=ORIENTED_EDGE('',*,*,#1788,.T.);
#2282=ORIENTED_EDGE('',*,*,#1747,.F.);
#2283=ORIENTED_EDGE('',*,*,#1786,.F.);
#2284=ORIENTED_EDGE('',*,*,#1789,.F.);
#2285=ORIENTED_EDGE('',*,*,#1790,.F.);
#2286=ORIENTED_EDGE('',*,*,#1791,.T.);
#2287=ORIENTED_EDGE('',*,*,#1772,.T.);
#2288=ORIENTED_EDGE('',*,*,#1792,.F.);
#2289=ORIENTED_EDGE('',*,*,#1784,.T.);
#2290=ORIENTED_EDGE('',*,*,#1781,.T.);
#2291=ORIENTED_EDGE('',*,*,#1793,.T.);
#2292=ORIENTED_EDGE('',*,*,#1773,.F.);
#2293=ORIENTED_EDGE('',*,*,#1791,.F.);
#2294=ORIENTED_EDGE('',*,*,#1754,.F.);
#2295=ORIENTED_EDGE('',*,*,#1748,.F.);
#2296=ORIENTED_EDGE('',*,*,#1788,.F.);
#2297=ORIENTED_EDGE('',*,*,#1774,.F.);
#2298=ORIENTED_EDGE('',*,*,#1793,.F.);
#2299=ORIENTED_EDGE('',*,*,#1780,.F.);
#2300=ORIENTED_EDGE('',*,*,#1766,.F.);
#2301=ORIENTED_EDGE('',*,*,#1760,.F.);
#2302=ORIENTED_EDGE('',*,*,#1794,.T.);
#2303=ORIENTED_EDGE('',*,*,#1795,.T.);
#2304=ORIENTED_EDGE('',*,*,#1796,.T.);
#2305=ORIENTED_EDGE('',*,*,#1795,.F.);
#2306=ORIENTED_EDGE('',*,*,#1797,.T.);
#2307=ORIENTED_EDGE('',*,*,#1794,.F.);
#2308=ORIENTED_EDGE('',*,*,#1798,.F.);
#2309=ORIENTED_EDGE('',*,*,#1799,.T.);
#2310=ORIENTED_EDGE('',*,*,#1796,.F.);
#2311=ORIENTED_EDGE('',*,*,#1799,.F.);
#2312=ORIENTED_EDGE('',*,*,#1800,.F.);
#2313=ORIENTED_EDGE('',*,*,#1801,.T.);
#2314=ORIENTED_EDGE('',*,*,#1798,.T.);
#2315=ORIENTED_EDGE('',*,*,#1801,.F.);
#2316=ORIENTED_EDGE('',*,*,#1802,.F.);
#2317=ORIENTED_EDGE('',*,*,#1803,.T.);
#2318=ORIENTED_EDGE('',*,*,#1800,.T.);
#2319=ORIENTED_EDGE('',*,*,#1803,.F.);
#2320=ORIENTED_EDGE('',*,*,#1802,.T.);
#2321=ORIENTED_EDGE('',*,*,#1779,.T.);
#2322=ORIENTED_EDGE('',*,*,#1783,.T.);
#2323=ORIENTED_EDGE('',*,*,#1792,.T.);
#2324=ORIENTED_EDGE('',*,*,#1790,.T.);
#2325=ORIENTED_EDGE('',*,*,#1771,.T.);
#2326=ORIENTED_EDGE('',*,*,#1777,.T.);
#2327=ORIENTED_EDGE('',*,*,#1787,.T.);
#2328=ORIENTED_EDGE('',*,*,#1804,.T.);
#2329=ORIENTED_EDGE('',*,*,#1805,.F.);
#2330=ORIENTED_EDGE('',*,*,#1806,.F.);
#2331=ORIENTED_EDGE('',*,*,#1804,.F.);
#2332=ORIENTED_EDGE('',*,*,#1789,.T.);
#2333=ORIENTED_EDGE('',*,*,#1785,.T.);
#2334=ORIENTED_EDGE('',*,*,#1745,.T.);
#2335=ORIENTED_EDGE('',*,*,#1751,.T.);
#2336=ORIENTED_EDGE('',*,*,#1753,.T.);
#2337=ORIENTED_EDGE('',*,*,#1757,.T.);
#2338=ORIENTED_EDGE('',*,*,#1759,.T.);
#2339=ORIENTED_EDGE('',*,*,#1763,.T.);
#2340=ORIENTED_EDGE('',*,*,#1765,.T.);
#2341=ORIENTED_EDGE('',*,*,#1769,.T.);
#2342=ORIENTED_EDGE('',*,*,#1797,.F.);
#2343=ORIENTED_EDGE('',*,*,#1807,.T.);
#2344=ORIENTED_EDGE('',*,*,#1805,.T.);
#2345=ORIENTED_EDGE('',*,*,#1806,.T.);
#2346=ORIENTED_EDGE('',*,*,#1807,.F.);
#2347=ORIENTED_EDGE('',*,*,#1808,.F.);
#2348=ORIENTED_EDGE('',*,*,#1809,.F.);
#2349=ORIENTED_EDGE('',*,*,#1810,.T.);
#2350=ORIENTED_EDGE('',*,*,#1811,.T.);
#2351=ORIENTED_EDGE('',*,*,#1812,.F.);
#2352=ORIENTED_EDGE('',*,*,#1813,.F.);
#2353=ORIENTED_EDGE('',*,*,#1814,.F.);
#2354=ORIENTED_EDGE('',*,*,#1813,.T.);
#2355=ORIENTED_EDGE('',*,*,#1815,.F.);
#2356=ORIENTED_EDGE('',*,*,#1816,.F.);
#2357=ORIENTED_EDGE('',*,*,#1815,.T.);
#2358=ORIENTED_EDGE('',*,*,#1812,.T.);
#2359=ORIENTED_EDGE('',*,*,#1817,.T.);
#2360=ORIENTED_EDGE('',*,*,#1818,.F.);
#2361=ORIENTED_EDGE('',*,*,#1819,.F.);
#2362=ORIENTED_EDGE('',*,*,#1820,.F.);
#2363=ORIENTED_EDGE('',*,*,#1819,.T.);
#2364=ORIENTED_EDGE('',*,*,#1821,.T.);
#2365=ORIENTED_EDGE('',*,*,#1822,.F.);
#2366=ORIENTED_EDGE('',*,*,#1821,.F.);
#2367=ORIENTED_EDGE('',*,*,#1818,.T.);
#2368=ORIENTED_EDGE('',*,*,#1823,.T.);
#2369=ORIENTED_EDGE('',*,*,#1824,.F.);
#2370=ORIENTED_EDGE('',*,*,#1825,.F.);
#2371=ORIENTED_EDGE('',*,*,#1826,.F.);
#2372=ORIENTED_EDGE('',*,*,#1825,.T.);
#2373=ORIENTED_EDGE('',*,*,#1827,.F.);
#2374=ORIENTED_EDGE('',*,*,#1828,.F.);
#2375=ORIENTED_EDGE('',*,*,#1827,.T.);
#2376=ORIENTED_EDGE('',*,*,#1824,.T.);
#2377=ORIENTED_EDGE('',*,*,#1829,.T.);
#2378=ORIENTED_EDGE('',*,*,#1830,.F.);
#2379=ORIENTED_EDGE('',*,*,#1831,.F.);
#2380=ORIENTED_EDGE('',*,*,#1832,.F.);
#2381=ORIENTED_EDGE('',*,*,#1831,.T.);
#2382=ORIENTED_EDGE('',*,*,#1833,.T.);
#2383=ORIENTED_EDGE('',*,*,#1834,.F.);
#2384=ORIENTED_EDGE('',*,*,#1835,.F.);
#2385=ORIENTED_EDGE('',*,*,#1836,.T.);
#2386=ORIENTED_EDGE('',*,*,#1837,.T.);
#2387=ORIENTED_EDGE('',*,*,#1838,.F.);
#2388=ORIENTED_EDGE('',*,*,#1839,.F.);
#2389=ORIENTED_EDGE('',*,*,#1840,.F.);
#2390=ORIENTED_EDGE('',*,*,#1839,.T.);
#2391=ORIENTED_EDGE('',*,*,#1841,.F.);
#2392=ORIENTED_EDGE('',*,*,#1842,.F.);
#2393=ORIENTED_EDGE('',*,*,#1833,.F.);
#2394=ORIENTED_EDGE('',*,*,#1830,.T.);
#2395=ORIENTED_EDGE('',*,*,#1843,.T.);
#2396=ORIENTED_EDGE('',*,*,#1844,.F.);
#2397=ORIENTED_EDGE('',*,*,#1845,.F.);
#2398=ORIENTED_EDGE('',*,*,#1846,.F.);
#2399=ORIENTED_EDGE('',*,*,#1845,.T.);
#2400=ORIENTED_EDGE('',*,*,#1847,.F.);
#2401=ORIENTED_EDGE('',*,*,#1848,.F.);
#2402=ORIENTED_EDGE('',*,*,#1849,.T.);
#2403=ORIENTED_EDGE('',*,*,#1809,.T.);
#2404=ORIENTED_EDGE('',*,*,#1850,.F.);
#2405=ORIENTED_EDGE('',*,*,#1841,.T.);
#2406=ORIENTED_EDGE('',*,*,#1838,.T.);
#2407=ORIENTED_EDGE('',*,*,#1851,.T.);
#2408=ORIENTED_EDGE('',*,*,#1810,.F.);
#2409=ORIENTED_EDGE('',*,*,#1849,.F.);
#2410=ORIENTED_EDGE('',*,*,#1852,.F.);
#2411=ORIENTED_EDGE('',*,*,#1853,.F.);
#2412=ORIENTED_EDGE('',*,*,#1854,.T.);
#2413=ORIENTED_EDGE('',*,*,#1835,.T.);
#2414=ORIENTED_EDGE('',*,*,#1855,.F.);
#2415=ORIENTED_EDGE('',*,*,#1847,.T.);
#2416=ORIENTED_EDGE('',*,*,#1844,.T.);
#2417=ORIENTED_EDGE('',*,*,#1856,.T.);
#2418=ORIENTED_EDGE('',*,*,#1836,.F.);
#2419=ORIENTED_EDGE('',*,*,#1854,.F.);
#2420=ORIENTED_EDGE('',*,*,#1817,.F.);
#2421=ORIENTED_EDGE('',*,*,#1811,.F.);
#2422=ORIENTED_EDGE('',*,*,#1851,.F.);
#2423=ORIENTED_EDGE('',*,*,#1837,.F.);
#2424=ORIENTED_EDGE('',*,*,#1856,.F.);
#2425=ORIENTED_EDGE('',*,*,#1843,.F.);
#2426=ORIENTED_EDGE('',*,*,#1829,.F.);
#2427=ORIENTED_EDGE('',*,*,#1823,.F.);
#2428=ORIENTED_EDGE('',*,*,#1857,.T.);
#2429=ORIENTED_EDGE('',*,*,#1858,.T.);
#2430=ORIENTED_EDGE('',*,*,#1859,.T.);
#2431=ORIENTED_EDGE('',*,*,#1858,.F.);
#2432=ORIENTED_EDGE('',*,*,#1860,.T.);
#2433=ORIENTED_EDGE('',*,*,#1857,.F.);
#2434=ORIENTED_EDGE('',*,*,#1861,.F.);
#2435=ORIENTED_EDGE('',*,*,#1862,.T.);
#2436=ORIENTED_EDGE('',*,*,#1859,.F.);
#2437=ORIENTED_EDGE('',*,*,#1862,.F.);
#2438=ORIENTED_EDGE('',*,*,#1863,.F.);
#2439=ORIENTED_EDGE('',*,*,#1864,.T.);
#2440=ORIENTED_EDGE('',*,*,#1861,.T.);
#2441=ORIENTED_EDGE('',*,*,#1864,.F.);
#2442=ORIENTED_EDGE('',*,*,#1865,.F.);
#2443=ORIENTED_EDGE('',*,*,#1866,.T.);
#2444=ORIENTED_EDGE('',*,*,#1863,.T.);
#2445=ORIENTED_EDGE('',*,*,#1866,.F.);
#2446=ORIENTED_EDGE('',*,*,#1865,.T.);
#2447=ORIENTED_EDGE('',*,*,#1842,.T.);
#2448=ORIENTED_EDGE('',*,*,#1846,.T.);
#2449=ORIENTED_EDGE('',*,*,#1855,.T.);
#2450=ORIENTED_EDGE('',*,*,#1853,.T.);
#2451=ORIENTED_EDGE('',*,*,#1834,.T.);
#2452=ORIENTED_EDGE('',*,*,#1840,.T.);
#2453=ORIENTED_EDGE('',*,*,#1850,.T.);
#2454=ORIENTED_EDGE('',*,*,#1867,.T.);
#2455=ORIENTED_EDGE('',*,*,#1868,.F.);
#2456=ORIENTED_EDGE('',*,*,#1869,.F.);
#2457=ORIENTED_EDGE('',*,*,#1867,.F.);
#2458=ORIENTED_EDGE('',*,*,#1852,.T.);
#2459=ORIENTED_EDGE('',*,*,#1848,.T.);
#2460=ORIENTED_EDGE('',*,*,#1808,.T.);
#2461=ORIENTED_EDGE('',*,*,#1814,.T.);
#2462=ORIENTED_EDGE('',*,*,#1816,.T.);
#2463=ORIENTED_EDGE('',*,*,#1820,.T.);
#2464=ORIENTED_EDGE('',*,*,#1822,.T.);
#2465=ORIENTED_EDGE('',*,*,#1826,.T.);
#2466=ORIENTED_EDGE('',*,*,#1828,.T.);
#2467=ORIENTED_EDGE('',*,*,#1832,.T.);
#2468=ORIENTED_EDGE('',*,*,#1860,.F.);
#2469=ORIENTED_EDGE('',*,*,#1870,.T.);
#2470=ORIENTED_EDGE('',*,*,#1868,.T.);
#2471=ORIENTED_EDGE('',*,*,#1869,.T.);
#2472=ORIENTED_EDGE('',*,*,#1870,.F.);
#2473=ORIENTED_EDGE('',*,*,#1871,.F.);
#2474=ORIENTED_EDGE('',*,*,#1872,.F.);
#2475=ORIENTED_EDGE('',*,*,#1873,.T.);
#2476=ORIENTED_EDGE('',*,*,#1874,.T.);
#2477=ORIENTED_EDGE('',*,*,#1875,.F.);
#2478=ORIENTED_EDGE('',*,*,#1876,.F.);
#2479=ORIENTED_EDGE('',*,*,#1877,.F.);
#2480=ORIENTED_EDGE('',*,*,#1876,.T.);
#2481=ORIENTED_EDGE('',*,*,#1878,.F.);
#2482=ORIENTED_EDGE('',*,*,#1879,.F.);
#2483=ORIENTED_EDGE('',*,*,#1878,.T.);
#2484=ORIENTED_EDGE('',*,*,#1875,.T.);
#2485=ORIENTED_EDGE('',*,*,#1880,.T.);
#2486=ORIENTED_EDGE('',*,*,#1881,.F.);
#2487=ORIENTED_EDGE('',*,*,#1882,.F.);
#2488=ORIENTED_EDGE('',*,*,#1883,.F.);
#2489=ORIENTED_EDGE('',*,*,#1882,.T.);
#2490=ORIENTED_EDGE('',*,*,#1884,.T.);
#2491=ORIENTED_EDGE('',*,*,#1885,.F.);
#2492=ORIENTED_EDGE('',*,*,#1884,.F.);
#2493=ORIENTED_EDGE('',*,*,#1881,.T.);
#2494=ORIENTED_EDGE('',*,*,#1886,.T.);
#2495=ORIENTED_EDGE('',*,*,#1887,.F.);
#2496=ORIENTED_EDGE('',*,*,#1888,.F.);
#2497=ORIENTED_EDGE('',*,*,#1889,.F.);
#2498=ORIENTED_EDGE('',*,*,#1888,.T.);
#2499=ORIENTED_EDGE('',*,*,#1890,.F.);
#2500=ORIENTED_EDGE('',*,*,#1891,.F.);
#2501=ORIENTED_EDGE('',*,*,#1890,.T.);
#2502=ORIENTED_EDGE('',*,*,#1887,.T.);
#2503=ORIENTED_EDGE('',*,*,#1892,.T.);
#2504=ORIENTED_EDGE('',*,*,#1893,.F.);
#2505=ORIENTED_EDGE('',*,*,#1894,.F.);
#2506=ORIENTED_EDGE('',*,*,#1895,.F.);
#2507=ORIENTED_EDGE('',*,*,#1894,.T.);
#2508=ORIENTED_EDGE('',*,*,#1896,.T.);
#2509=ORIENTED_EDGE('',*,*,#1897,.F.);
#2510=ORIENTED_EDGE('',*,*,#1898,.F.);
#2511=ORIENTED_EDGE('',*,*,#1899,.T.);
#2512=ORIENTED_EDGE('',*,*,#1900,.T.);
#2513=ORIENTED_EDGE('',*,*,#1901,.F.);
#2514=ORIENTED_EDGE('',*,*,#1902,.F.);
#2515=ORIENTED_EDGE('',*,*,#1903,.F.);
#2516=ORIENTED_EDGE('',*,*,#1902,.T.);
#2517=ORIENTED_EDGE('',*,*,#1904,.F.);
#2518=ORIENTED_EDGE('',*,*,#1905,.F.);
#2519=ORIENTED_EDGE('',*,*,#1896,.F.);
#2520=ORIENTED_EDGE('',*,*,#1893,.T.);
#2521=ORIENTED_EDGE('',*,*,#1906,.T.);
#2522=ORIENTED_EDGE('',*,*,#1907,.F.);
#2523=ORIENTED_EDGE('',*,*,#1908,.F.);
#2524=ORIENTED_EDGE('',*,*,#1909,.F.);
#2525=ORIENTED_EDGE('',*,*,#1908,.T.);
#2526=ORIENTED_EDGE('',*,*,#1910,.F.);
#2527=ORIENTED_EDGE('',*,*,#1911,.F.);
#2528=ORIENTED_EDGE('',*,*,#1912,.T.);
#2529=ORIENTED_EDGE('',*,*,#1872,.T.);
#2530=ORIENTED_EDGE('',*,*,#1913,.F.);
#2531=ORIENTED_EDGE('',*,*,#1904,.T.);
#2532=ORIENTED_EDGE('',*,*,#1901,.T.);
#2533=ORIENTED_EDGE('',*,*,#1914,.T.);
#2534=ORIENTED_EDGE('',*,*,#1873,.F.);
#2535=ORIENTED_EDGE('',*,*,#1912,.F.);
#2536=ORIENTED_EDGE('',*,*,#1915,.F.);
#2537=ORIENTED_EDGE('',*,*,#1916,.F.);
#2538=ORIENTED_EDGE('',*,*,#1917,.T.);
#2539=ORIENTED_EDGE('',*,*,#1898,.T.);
#2540=ORIENTED_EDGE('',*,*,#1918,.F.);
#2541=ORIENTED_EDGE('',*,*,#1910,.T.);
#2542=ORIENTED_EDGE('',*,*,#1907,.T.);
#2543=ORIENTED_EDGE('',*,*,#1919,.T.);
#2544=ORIENTED_EDGE('',*,*,#1899,.F.);
#2545=ORIENTED_EDGE('',*,*,#1917,.F.);
#2546=ORIENTED_EDGE('',*,*,#1880,.F.);
#2547=ORIENTED_EDGE('',*,*,#1874,.F.);
#2548=ORIENTED_EDGE('',*,*,#1914,.F.);
#2549=ORIENTED_EDGE('',*,*,#1900,.F.);
#2550=ORIENTED_EDGE('',*,*,#1919,.F.);
#2551=ORIENTED_EDGE('',*,*,#1906,.F.);
#2552=ORIENTED_EDGE('',*,*,#1892,.F.);
#2553=ORIENTED_EDGE('',*,*,#1886,.F.);
#2554=ORIENTED_EDGE('',*,*,#1920,.T.);
#2555=ORIENTED_EDGE('',*,*,#1921,.T.);
#2556=ORIENTED_EDGE('',*,*,#1922,.T.);
#2557=ORIENTED_EDGE('',*,*,#1921,.F.);
#2558=ORIENTED_EDGE('',*,*,#1923,.T.);
#2559=ORIENTED_EDGE('',*,*,#1920,.F.);
#2560=ORIENTED_EDGE('',*,*,#1924,.F.);
#2561=ORIENTED_EDGE('',*,*,#1925,.T.);
#2562=ORIENTED_EDGE('',*,*,#1922,.F.);
#2563=ORIENTED_EDGE('',*,*,#1925,.F.);
#2564=ORIENTED_EDGE('',*,*,#1926,.F.);
#2565=ORIENTED_EDGE('',*,*,#1927,.T.);
#2566=ORIENTED_EDGE('',*,*,#1924,.T.);
#2567=ORIENTED_EDGE('',*,*,#1927,.F.);
#2568=ORIENTED_EDGE('',*,*,#1928,.F.);
#2569=ORIENTED_EDGE('',*,*,#1929,.T.);
#2570=ORIENTED_EDGE('',*,*,#1926,.T.);
#2571=ORIENTED_EDGE('',*,*,#1929,.F.);
#2572=ORIENTED_EDGE('',*,*,#1928,.T.);
#2573=ORIENTED_EDGE('',*,*,#1905,.T.);
#2574=ORIENTED_EDGE('',*,*,#1909,.T.);
#2575=ORIENTED_EDGE('',*,*,#1918,.T.);
#2576=ORIENTED_EDGE('',*,*,#1916,.T.);
#2577=ORIENTED_EDGE('',*,*,#1897,.T.);
#2578=ORIENTED_EDGE('',*,*,#1903,.T.);
#2579=ORIENTED_EDGE('',*,*,#1913,.T.);
#2580=ORIENTED_EDGE('',*,*,#1930,.T.);
#2581=ORIENTED_EDGE('',*,*,#1931,.F.);
#2582=ORIENTED_EDGE('',*,*,#1932,.F.);
#2583=ORIENTED_EDGE('',*,*,#1930,.F.);
#2584=ORIENTED_EDGE('',*,*,#1915,.T.);
#2585=ORIENTED_EDGE('',*,*,#1911,.T.);
#2586=ORIENTED_EDGE('',*,*,#1871,.T.);
#2587=ORIENTED_EDGE('',*,*,#1877,.T.);
#2588=ORIENTED_EDGE('',*,*,#1879,.T.);
#2589=ORIENTED_EDGE('',*,*,#1883,.T.);
#2590=ORIENTED_EDGE('',*,*,#1885,.T.);
#2591=ORIENTED_EDGE('',*,*,#1889,.T.);
#2592=ORIENTED_EDGE('',*,*,#1891,.T.);
#2593=ORIENTED_EDGE('',*,*,#1895,.T.);
#2594=ORIENTED_EDGE('',*,*,#1923,.F.);
#2595=ORIENTED_EDGE('',*,*,#1933,.T.);
#2596=ORIENTED_EDGE('',*,*,#1931,.T.);
#2597=ORIENTED_EDGE('',*,*,#1932,.T.);
#2598=ORIENTED_EDGE('',*,*,#1933,.F.);
#2599=ORIENTED_EDGE('',*,*,#1934,.F.);
#2600=ORIENTED_EDGE('',*,*,#1935,.F.);
#2601=ORIENTED_EDGE('',*,*,#1936,.T.);
#2602=ORIENTED_EDGE('',*,*,#1937,.T.);
#2603=ORIENTED_EDGE('',*,*,#1938,.F.);
#2604=ORIENTED_EDGE('',*,*,#1939,.F.);
#2605=ORIENTED_EDGE('',*,*,#1940,.F.);
#2606=ORIENTED_EDGE('',*,*,#1939,.T.);
#2607=ORIENTED_EDGE('',*,*,#1941,.F.);
#2608=ORIENTED_EDGE('',*,*,#1942,.F.);
#2609=ORIENTED_EDGE('',*,*,#1941,.T.);
#2610=ORIENTED_EDGE('',*,*,#1938,.T.);
#2611=ORIENTED_EDGE('',*,*,#1943,.T.);
#2612=ORIENTED_EDGE('',*,*,#1944,.F.);
#2613=ORIENTED_EDGE('',*,*,#1945,.F.);
#2614=ORIENTED_EDGE('',*,*,#1946,.F.);
#2615=ORIENTED_EDGE('',*,*,#1945,.T.);
#2616=ORIENTED_EDGE('',*,*,#1947,.T.);
#2617=ORIENTED_EDGE('',*,*,#1948,.F.);
#2618=ORIENTED_EDGE('',*,*,#1947,.F.);
#2619=ORIENTED_EDGE('',*,*,#1944,.T.);
#2620=ORIENTED_EDGE('',*,*,#1949,.T.);
#2621=ORIENTED_EDGE('',*,*,#1950,.F.);
#2622=ORIENTED_EDGE('',*,*,#1951,.F.);
#2623=ORIENTED_EDGE('',*,*,#1952,.F.);
#2624=ORIENTED_EDGE('',*,*,#1951,.T.);
#2625=ORIENTED_EDGE('',*,*,#1953,.F.);
#2626=ORIENTED_EDGE('',*,*,#1954,.F.);
#2627=ORIENTED_EDGE('',*,*,#1953,.T.);
#2628=ORIENTED_EDGE('',*,*,#1950,.T.);
#2629=ORIENTED_EDGE('',*,*,#1955,.T.);
#2630=ORIENTED_EDGE('',*,*,#1956,.F.);
#2631=ORIENTED_EDGE('',*,*,#1957,.F.);
#2632=ORIENTED_EDGE('',*,*,#1958,.F.);
#2633=ORIENTED_EDGE('',*,*,#1957,.T.);
#2634=ORIENTED_EDGE('',*,*,#1959,.T.);
#2635=ORIENTED_EDGE('',*,*,#1960,.F.);
#2636=ORIENTED_EDGE('',*,*,#1961,.F.);
#2637=ORIENTED_EDGE('',*,*,#1962,.T.);
#2638=ORIENTED_EDGE('',*,*,#1963,.T.);
#2639=ORIENTED_EDGE('',*,*,#1964,.F.);
#2640=ORIENTED_EDGE('',*,*,#1965,.F.);
#2641=ORIENTED_EDGE('',*,*,#1966,.F.);
#2642=ORIENTED_EDGE('',*,*,#1965,.T.);
#2643=ORIENTED_EDGE('',*,*,#1967,.F.);
#2644=ORIENTED_EDGE('',*,*,#1968,.F.);
#2645=ORIENTED_EDGE('',*,*,#1959,.F.);
#2646=ORIENTED_EDGE('',*,*,#1956,.T.);
#2647=ORIENTED_EDGE('',*,*,#1969,.T.);
#2648=ORIENTED_EDGE('',*,*,#1970,.F.);
#2649=ORIENTED_EDGE('',*,*,#1971,.F.);
#2650=ORIENTED_EDGE('',*,*,#1972,.F.);
#2651=ORIENTED_EDGE('',*,*,#1971,.T.);
#2652=ORIENTED_EDGE('',*,*,#1973,.F.);
#2653=ORIENTED_EDGE('',*,*,#1974,.F.);
#2654=ORIENTED_EDGE('',*,*,#1975,.T.);
#2655=ORIENTED_EDGE('',*,*,#1935,.T.);
#2656=ORIENTED_EDGE('',*,*,#1976,.F.);
#2657=ORIENTED_EDGE('',*,*,#1967,.T.);
#2658=ORIENTED_EDGE('',*,*,#1964,.T.);
#2659=ORIENTED_EDGE('',*,*,#1977,.T.);
#2660=ORIENTED_EDGE('',*,*,#1936,.F.);
#2661=ORIENTED_EDGE('',*,*,#1975,.F.);
#2662=ORIENTED_EDGE('',*,*,#1978,.F.);
#2663=ORIENTED_EDGE('',*,*,#1979,.F.);
#2664=ORIENTED_EDGE('',*,*,#1980,.T.);
#2665=ORIENTED_EDGE('',*,*,#1961,.T.);
#2666=ORIENTED_EDGE('',*,*,#1981,.F.);
#2667=ORIENTED_EDGE('',*,*,#1973,.T.);
#2668=ORIENTED_EDGE('',*,*,#1970,.T.);
#2669=ORIENTED_EDGE('',*,*,#1982,.T.);
#2670=ORIENTED_EDGE('',*,*,#1962,.F.);
#2671=ORIENTED_EDGE('',*,*,#1980,.F.);
#2672=ORIENTED_EDGE('',*,*,#1943,.F.);
#2673=ORIENTED_EDGE('',*,*,#1937,.F.);
#2674=ORIENTED_EDGE('',*,*,#1977,.F.);
#2675=ORIENTED_EDGE('',*,*,#1963,.F.);
#2676=ORIENTED_EDGE('',*,*,#1982,.F.);
#2677=ORIENTED_EDGE('',*,*,#1969,.F.);
#2678=ORIENTED_EDGE('',*,*,#1955,.F.);
#2679=ORIENTED_EDGE('',*,*,#1949,.F.);
#2680=ORIENTED_EDGE('',*,*,#1983,.T.);
#2681=ORIENTED_EDGE('',*,*,#1984,.T.);
#2682=ORIENTED_EDGE('',*,*,#1985,.T.);
#2683=ORIENTED_EDGE('',*,*,#1984,.F.);
#2684=ORIENTED_EDGE('',*,*,#1986,.T.);
#2685=ORIENTED_EDGE('',*,*,#1983,.F.);
#2686=ORIENTED_EDGE('',*,*,#1987,.F.);
#2687=ORIENTED_EDGE('',*,*,#1988,.T.);
#2688=ORIENTED_EDGE('',*,*,#1985,.F.);
#2689=ORIENTED_EDGE('',*,*,#1988,.F.);
#2690=ORIENTED_EDGE('',*,*,#1989,.F.);
#2691=ORIENTED_EDGE('',*,*,#1990,.T.);
#2692=ORIENTED_EDGE('',*,*,#1987,.T.);
#2693=ORIENTED_EDGE('',*,*,#1990,.F.);
#2694=ORIENTED_EDGE('',*,*,#1991,.F.);
#2695=ORIENTED_EDGE('',*,*,#1992,.T.);
#2696=ORIENTED_EDGE('',*,*,#1989,.T.);
#2697=ORIENTED_EDGE('',*,*,#1992,.F.);
#2698=ORIENTED_EDGE('',*,*,#1991,.T.);
#2699=ORIENTED_EDGE('',*,*,#1968,.T.);
#2700=ORIENTED_EDGE('',*,*,#1972,.T.);
#2701=ORIENTED_EDGE('',*,*,#1981,.T.);
#2702=ORIENTED_EDGE('',*,*,#1979,.T.);
#2703=ORIENTED_EDGE('',*,*,#1960,.T.);
#2704=ORIENTED_EDGE('',*,*,#1966,.T.);
#2705=ORIENTED_EDGE('',*,*,#1976,.T.);
#2706=ORIENTED_EDGE('',*,*,#1993,.T.);
#2707=ORIENTED_EDGE('',*,*,#1994,.F.);
#2708=ORIENTED_EDGE('',*,*,#1995,.F.);
#2709=ORIENTED_EDGE('',*,*,#1993,.F.);
#2710=ORIENTED_EDGE('',*,*,#1978,.T.);
#2711=ORIENTED_EDGE('',*,*,#1974,.T.);
#2712=ORIENTED_EDGE('',*,*,#1934,.T.);
#2713=ORIENTED_EDGE('',*,*,#1940,.T.);
#2714=ORIENTED_EDGE('',*,*,#1942,.T.);
#2715=ORIENTED_EDGE('',*,*,#1946,.T.);
#2716=ORIENTED_EDGE('',*,*,#1948,.T.);
#2717=ORIENTED_EDGE('',*,*,#1952,.T.);
#2718=ORIENTED_EDGE('',*,*,#1954,.T.);
#2719=ORIENTED_EDGE('',*,*,#1958,.T.);
#2720=ORIENTED_EDGE('',*,*,#1986,.F.);
#2721=ORIENTED_EDGE('',*,*,#1996,.T.);
#2722=ORIENTED_EDGE('',*,*,#1994,.T.);
#2723=ORIENTED_EDGE('',*,*,#1995,.T.);
#2724=ORIENTED_EDGE('',*,*,#1996,.F.);
#2725=ORIENTED_EDGE('',*,*,#1997,.F.);
#2726=ORIENTED_EDGE('',*,*,#1998,.F.);
#2727=ORIENTED_EDGE('',*,*,#1999,.F.);
#2728=ORIENTED_EDGE('',*,*,#2000,.F.);
#2729=ORIENTED_EDGE('',*,*,#2001,.F.);
#2730=ORIENTED_EDGE('',*,*,#2000,.T.);
#2731=ORIENTED_EDGE('',*,*,#2002,.F.);
#2732=ORIENTED_EDGE('',*,*,#2003,.F.);
#2733=ORIENTED_EDGE('',*,*,#2004,.F.);
#2734=ORIENTED_EDGE('',*,*,#2003,.T.);
#2735=ORIENTED_EDGE('',*,*,#2005,.F.);
#2736=ORIENTED_EDGE('',*,*,#2006,.F.);
#2737=ORIENTED_EDGE('',*,*,#2007,.F.);
#2738=ORIENTED_EDGE('',*,*,#2005,.T.);
#2739=ORIENTED_EDGE('',*,*,#2002,.T.);
#2740=ORIENTED_EDGE('',*,*,#1999,.T.);
#2741=ORIENTED_EDGE('',*,*,#2006,.T.);
#2742=ORIENTED_EDGE('',*,*,#2007,.T.);
#2743=ORIENTED_EDGE('',*,*,#1998,.T.);
#2744=ORIENTED_EDGE('',*,*,#2008,.T.);
#2745=ORIENTED_EDGE('',*,*,#2009,.T.);
#2746=ORIENTED_EDGE('',*,*,#2010,.T.);
#2747=ORIENTED_EDGE('',*,*,#2011,.T.);
#2748=ORIENTED_EDGE('',*,*,#2012,.T.);
#2749=ORIENTED_EDGE('',*,*,#2013,.T.);
#2750=ORIENTED_EDGE('',*,*,#2014,.T.);
#2751=ORIENTED_EDGE('',*,*,#2004,.T.);
#2752=ORIENTED_EDGE('',*,*,#2012,.F.);
#2753=ORIENTED_EDGE('',*,*,#2015,.F.);
#2754=ORIENTED_EDGE('',*,*,#2016,.F.);
#2755=ORIENTED_EDGE('',*,*,#2017,.F.);
#2756=ORIENTED_EDGE('',*,*,#2008,.F.);
#2757=ORIENTED_EDGE('',*,*,#1997,.T.);
#2758=ORIENTED_EDGE('',*,*,#2001,.T.);
#2759=ORIENTED_EDGE('',*,*,#2016,.T.);
#2760=ORIENTED_EDGE('',*,*,#2018,.T.);
#2761=ORIENTED_EDGE('',*,*,#2019,.T.);
#2762=ORIENTED_EDGE('',*,*,#2020,.T.);
#2763=ORIENTED_EDGE('',*,*,#2021,.T.);
#2764=ORIENTED_EDGE('',*,*,#2022,.T.);
#2765=ORIENTED_EDGE('',*,*,#2015,.T.);
#2766=ORIENTED_EDGE('',*,*,#2011,.F.);
#2767=ORIENTED_EDGE('',*,*,#2023,.T.);
#2768=ORIENTED_EDGE('',*,*,#2018,.F.);
#2769=ORIENTED_EDGE('',*,*,#2017,.T.);
#2770=ORIENTED_EDGE('',*,*,#2020,.F.);
#2771=ORIENTED_EDGE('',*,*,#2024,.F.);
#2772=ORIENTED_EDGE('',*,*,#2009,.F.);
#2773=ORIENTED_EDGE('',*,*,#2022,.F.);
#2774=ORIENTED_EDGE('',*,*,#2025,.T.);
#2775=ORIENTED_EDGE('',*,*,#2013,.F.);
#2776=ORIENTED_EDGE('',*,*,#2025,.F.);
#2777=ORIENTED_EDGE('',*,*,#2021,.F.);
#2778=ORIENTED_EDGE('',*,*,#2026,.T.);
#2779=ORIENTED_EDGE('',*,*,#2014,.F.);
#2780=ORIENTED_EDGE('',*,*,#2026,.F.);
#2781=ORIENTED_EDGE('',*,*,#2010,.F.);
#2782=ORIENTED_EDGE('',*,*,#2024,.T.);
#2783=ORIENTED_EDGE('',*,*,#2019,.F.);
#2784=ORIENTED_EDGE('',*,*,#2023,.F.);
#2785=ORIENTED_EDGE('',*,*,#2027,.F.);
#2786=ORIENTED_EDGE('',*,*,#2028,.T.);
#2787=ORIENTED_EDGE('',*,*,#2029,.F.);
#2788=ORIENTED_EDGE('',*,*,#2030,.F.);
#2789=ORIENTED_EDGE('',*,*,#2031,.F.);
#2790=ORIENTED_EDGE('',*,*,#2030,.T.);
#2791=ORIENTED_EDGE('',*,*,#2032,.F.);
#2792=ORIENTED_EDGE('',*,*,#2033,.F.);
#2793=ORIENTED_EDGE('',*,*,#2034,.F.);
#2794=ORIENTED_EDGE('',*,*,#2033,.T.);
#2795=ORIENTED_EDGE('',*,*,#2035,.F.);
#2796=ORIENTED_EDGE('',*,*,#2036,.F.);
#2797=ORIENTED_EDGE('',*,*,#2037,.T.);
#2798=ORIENTED_EDGE('',*,*,#2035,.T.);
#2799=ORIENTED_EDGE('',*,*,#2032,.T.);
#2800=ORIENTED_EDGE('',*,*,#2029,.T.);
#2801=ORIENTED_EDGE('',*,*,#2034,.T.);
#2802=ORIENTED_EDGE('',*,*,#2038,.F.);
#2803=ORIENTED_EDGE('',*,*,#2039,.F.);
#2804=ORIENTED_EDGE('',*,*,#2040,.F.);
#2805=ORIENTED_EDGE('',*,*,#2041,.F.);
#2806=ORIENTED_EDGE('',*,*,#2042,.F.);
#2807=ORIENTED_EDGE('',*,*,#2027,.T.);
#2808=ORIENTED_EDGE('',*,*,#2031,.T.);
#2809=ORIENTED_EDGE('',*,*,#2043,.F.);
#2810=ORIENTED_EDGE('',*,*,#2044,.T.);
#2811=ORIENTED_EDGE('',*,*,#2045,.F.);
#2812=ORIENTED_EDGE('',*,*,#2044,.F.);
#2813=ORIENTED_EDGE('',*,*,#2046,.F.);
#2814=ORIENTED_EDGE('',*,*,#2047,.F.);
#2815=ORIENTED_EDGE('',*,*,#2048,.F.);
#2816=ORIENTED_EDGE('',*,*,#2049,.F.);
#2817=ORIENTED_EDGE('',*,*,#2050,.F.);
#2818=ORIENTED_EDGE('',*,*,#2051,.F.);
#2819=ORIENTED_EDGE('',*,*,#2052,.F.);
#2820=ORIENTED_EDGE('',*,*,#2053,.T.);
#2821=ORIENTED_EDGE('',*,*,#2054,.F.);
#2822=ORIENTED_EDGE('',*,*,#2053,.F.);
#2823=ORIENTED_EDGE('',*,*,#2055,.F.);
#2824=ORIENTED_EDGE('',*,*,#2047,.T.);
#2825=ORIENTED_EDGE('',*,*,#2049,.T.);
#2826=ORIENTED_EDGE('',*,*,#2056,.F.);
#2827=ORIENTED_EDGE('',*,*,#2057,.T.);
#2828=ORIENTED_EDGE('',*,*,#2058,.T.);
#2829=ORIENTED_EDGE('',*,*,#2059,.T.);
#2830=ORIENTED_EDGE('',*,*,#2060,.F.);
#2831=ORIENTED_EDGE('',*,*,#2061,.F.);
#2832=ORIENTED_EDGE('',*,*,#2062,.T.);
#2833=ORIENTED_EDGE('',*,*,#2063,.F.);
#2834=ORIENTED_EDGE('',*,*,#2064,.F.);
#2835=ORIENTED_EDGE('',*,*,#2057,.F.);
#2836=ORIENTED_EDGE('',*,*,#2065,.F.);
#2837=ORIENTED_EDGE('',*,*,#2066,.T.);
#2838=ORIENTED_EDGE('',*,*,#2067,.T.);
#2839=ORIENTED_EDGE('',*,*,#2068,.F.);
#2840=ORIENTED_EDGE('',*,*,#2063,.T.);
#2841=ORIENTED_EDGE('',*,*,#2069,.T.);
#2842=ORIENTED_EDGE('',*,*,#2066,.F.);
#2843=ORIENTED_EDGE('',*,*,#2070,.F.);
#2844=ORIENTED_EDGE('',*,*,#2058,.F.);
#2845=ORIENTED_EDGE('',*,*,#2067,.F.);
#2846=ORIENTED_EDGE('',*,*,#2069,.F.);
#2847=ORIENTED_EDGE('',*,*,#2062,.F.);
#2848=ORIENTED_EDGE('',*,*,#2071,.F.);
#2849=ORIENTED_EDGE('',*,*,#2072,.T.);
#2850=ORIENTED_EDGE('',*,*,#2073,.F.);
#2851=ORIENTED_EDGE('',*,*,#2074,.F.);
#2852=ORIENTED_EDGE('',*,*,#2043,.T.);
#2853=ORIENTED_EDGE('',*,*,#2051,.T.);
#2854=ORIENTED_EDGE('',*,*,#2075,.F.);
#2855=ORIENTED_EDGE('',*,*,#2072,.F.);
#2856=ORIENTED_EDGE('',*,*,#2076,.F.);
#2857=ORIENTED_EDGE('',*,*,#2077,.T.);
#2858=ORIENTED_EDGE('',*,*,#2078,.F.);
#2859=ORIENTED_EDGE('',*,*,#2041,.T.);
#2860=ORIENTED_EDGE('',*,*,#2079,.F.);
#2861=ORIENTED_EDGE('',*,*,#2045,.T.);
#2862=ORIENTED_EDGE('',*,*,#2080,.T.);
#2863=ORIENTED_EDGE('',*,*,#2081,.T.);
#2864=ORIENTED_EDGE('',*,*,#2038,.T.);
#2865=ORIENTED_EDGE('',*,*,#2036,.T.);
#2866=ORIENTED_EDGE('',*,*,#2037,.F.);
#2867=ORIENTED_EDGE('',*,*,#2028,.F.);
#2868=ORIENTED_EDGE('',*,*,#2042,.T.);
#2869=ORIENTED_EDGE('',*,*,#2078,.T.);
#2870=ORIENTED_EDGE('',*,*,#2082,.T.);
#2871=ORIENTED_EDGE('',*,*,#2073,.T.);
#2872=ORIENTED_EDGE('',*,*,#2075,.T.);
#2873=ORIENTED_EDGE('',*,*,#2050,.T.);
#2874=ORIENTED_EDGE('',*,*,#2054,.T.);
#2875=ORIENTED_EDGE('',*,*,#2046,.T.);
#2876=ORIENTED_EDGE('',*,*,#2060,.T.);
#2877=ORIENTED_EDGE('',*,*,#2083,.T.);
#2878=ORIENTED_EDGE('',*,*,#2074,.T.);
#2879=ORIENTED_EDGE('',*,*,#2082,.F.);
#2880=ORIENTED_EDGE('',*,*,#2077,.F.);
#2881=ORIENTED_EDGE('',*,*,#2084,.F.);
#2882=ORIENTED_EDGE('',*,*,#2085,.T.);
#2883=ORIENTED_EDGE('',*,*,#2064,.T.);
#2884=ORIENTED_EDGE('',*,*,#2068,.T.);
#2885=ORIENTED_EDGE('',*,*,#2065,.T.);
#2886=ORIENTED_EDGE('',*,*,#2056,.T.);
#2887=ORIENTED_EDGE('',*,*,#2048,.T.);
#2888=ORIENTED_EDGE('',*,*,#2055,.T.);
#2889=ORIENTED_EDGE('',*,*,#2052,.T.);
#2890=ORIENTED_EDGE('',*,*,#2076,.T.);
#2891=ORIENTED_EDGE('',*,*,#2071,.T.);
#2892=ORIENTED_EDGE('',*,*,#2084,.T.);
#2893=ORIENTED_EDGE('',*,*,#2079,.T.);
#2894=ORIENTED_EDGE('',*,*,#2040,.T.);
#2895=ORIENTED_EDGE('',*,*,#2086,.T.);
#2896=ORIENTED_EDGE('',*,*,#2087,.T.);
#2897=ORIENTED_EDGE('',*,*,#2083,.F.);
#2898=ORIENTED_EDGE('',*,*,#2059,.F.);
#2899=ORIENTED_EDGE('',*,*,#2070,.T.);
#2900=ORIENTED_EDGE('',*,*,#2088,.T.);
#2901=ORIENTED_EDGE('',*,*,#2086,.F.);
#2902=ORIENTED_EDGE('',*,*,#2039,.T.);
#2903=ORIENTED_EDGE('',*,*,#2081,.F.);
#2904=ORIENTED_EDGE('',*,*,#2080,.F.);
#2905=ORIENTED_EDGE('',*,*,#2087,.F.);
#2906=ORIENTED_EDGE('',*,*,#2061,.T.);
#2907=ORIENTED_EDGE('',*,*,#2085,.F.);
#2908=ORIENTED_EDGE('',*,*,#2088,.F.);
#2909=ORIENTED_EDGE('',*,*,#2089,.F.);
#2910=ORIENTED_EDGE('',*,*,#2090,.F.);
#2911=ORIENTED_EDGE('',*,*,#2091,.T.);
#2912=ORIENTED_EDGE('',*,*,#2092,.F.);
#2913=ORIENTED_EDGE('',*,*,#2093,.F.);
#2914=ORIENTED_EDGE('',*,*,#2092,.T.);
#2915=ORIENTED_EDGE('',*,*,#2094,.T.);
#2916=ORIENTED_EDGE('',*,*,#2095,.F.);
#2917=ORIENTED_EDGE('',*,*,#2096,.F.);
#2918=ORIENTED_EDGE('',*,*,#2095,.T.);
#2919=ORIENTED_EDGE('',*,*,#2097,.T.);
#2920=ORIENTED_EDGE('',*,*,#2098,.F.);
#2921=ORIENTED_EDGE('',*,*,#2099,.F.);
#2922=ORIENTED_EDGE('',*,*,#2097,.F.);
#2923=ORIENTED_EDGE('',*,*,#2094,.F.);
#2924=ORIENTED_EDGE('',*,*,#2091,.F.);
#2925=ORIENTED_EDGE('',*,*,#2089,.T.);
#2926=ORIENTED_EDGE('',*,*,#2093,.T.);
#2927=ORIENTED_EDGE('',*,*,#2096,.T.);
#2928=ORIENTED_EDGE('',*,*,#2100,.F.);
#2929=ORIENTED_EDGE('',*,*,#2101,.F.);
#2930=ORIENTED_EDGE('',*,*,#2102,.F.);
#2931=ORIENTED_EDGE('',*,*,#2103,.F.);
#2932=ORIENTED_EDGE('',*,*,#2104,.F.);
#2933=ORIENTED_EDGE('',*,*,#2102,.T.);
#2934=ORIENTED_EDGE('',*,*,#2105,.T.);
#2935=ORIENTED_EDGE('',*,*,#2106,.T.);
#2936=ORIENTED_EDGE('',*,*,#2107,.T.);
#2937=ORIENTED_EDGE('',*,*,#2108,.T.);
#2938=ORIENTED_EDGE('',*,*,#2109,.T.);
#2939=ORIENTED_EDGE('',*,*,#2103,.T.);
#2940=ORIENTED_EDGE('',*,*,#2107,.F.);
#2941=ORIENTED_EDGE('',*,*,#2110,.F.);
#2942=ORIENTED_EDGE('',*,*,#2111,.F.);
#2943=ORIENTED_EDGE('',*,*,#2090,.T.);
#2944=ORIENTED_EDGE('',*,*,#2104,.T.);
#2945=ORIENTED_EDGE('',*,*,#2111,.T.);
#2946=ORIENTED_EDGE('',*,*,#2112,.T.);
#2947=ORIENTED_EDGE('',*,*,#2113,.T.);
#2948=ORIENTED_EDGE('',*,*,#2100,.T.);
#2949=ORIENTED_EDGE('',*,*,#2098,.T.);
#2950=ORIENTED_EDGE('',*,*,#2099,.T.);
#2951=ORIENTED_EDGE('',*,*,#2114,.T.);
#2952=ORIENTED_EDGE('',*,*,#2115,.T.);
#2953=ORIENTED_EDGE('',*,*,#2101,.T.);
#2954=ORIENTED_EDGE('',*,*,#2113,.F.);
#2955=ORIENTED_EDGE('',*,*,#2116,.T.);
#2956=ORIENTED_EDGE('',*,*,#2105,.F.);
#2957=ORIENTED_EDGE('',*,*,#2109,.F.);
#2958=ORIENTED_EDGE('',*,*,#2117,.T.);
#2959=ORIENTED_EDGE('',*,*,#2115,.F.);
#2960=ORIENTED_EDGE('',*,*,#2117,.F.);
#2961=ORIENTED_EDGE('',*,*,#2108,.F.);
#2962=ORIENTED_EDGE('',*,*,#2118,.T.);
#2963=ORIENTED_EDGE('',*,*,#2114,.F.);
#2964=ORIENTED_EDGE('',*,*,#2118,.F.);
#2965=ORIENTED_EDGE('',*,*,#2112,.F.);
#2966=ORIENTED_EDGE('',*,*,#2110,.T.);
#2967=ORIENTED_EDGE('',*,*,#2106,.F.);
#2968=ORIENTED_EDGE('',*,*,#2116,.F.);
#2969=ORIENTED_EDGE('',*,*,#2119,.F.);
#2970=ORIENTED_EDGE('',*,*,#2120,.T.);
#2971=ORIENTED_EDGE('',*,*,#2121,.T.);
#2972=ORIENTED_EDGE('',*,*,#2122,.F.);
#2973=ORIENTED_EDGE('',*,*,#2123,.F.);
#2974=ORIENTED_EDGE('',*,*,#2124,.T.);
#2975=ORIENTED_EDGE('',*,*,#2125,.T.);
#2976=ORIENTED_EDGE('',*,*,#2120,.F.);
#2977=ORIENTED_EDGE('',*,*,#2126,.F.);
#2978=ORIENTED_EDGE('',*,*,#2127,.T.);
#2979=ORIENTED_EDGE('',*,*,#2128,.T.);
#2980=ORIENTED_EDGE('',*,*,#2124,.F.);
#2981=ORIENTED_EDGE('',*,*,#2129,.F.);
#2982=ORIENTED_EDGE('',*,*,#2121,.F.);
#2983=ORIENTED_EDGE('',*,*,#2125,.F.);
#2984=ORIENTED_EDGE('',*,*,#2128,.F.);
#2985=ORIENTED_EDGE('',*,*,#2126,.T.);
#2986=ORIENTED_EDGE('',*,*,#2123,.T.);
#2987=ORIENTED_EDGE('',*,*,#2119,.T.);
#2988=ORIENTED_EDGE('',*,*,#2130,.F.);
#2989=ORIENTED_EDGE('',*,*,#2131,.T.);
#2990=ORIENTED_EDGE('',*,*,#2132,.F.);
#2991=ORIENTED_EDGE('',*,*,#2133,.F.);
#2992=ORIENTED_EDGE('',*,*,#2134,.F.);
#2993=ORIENTED_EDGE('',*,*,#2135,.F.);
#2994=ORIENTED_EDGE('',*,*,#2136,.F.);
#2995=ORIENTED_EDGE('',*,*,#2137,.F.);
#2996=ORIENTED_EDGE('',*,*,#2138,.F.);
#2997=ORIENTED_EDGE('',*,*,#2139,.F.);
#2998=ORIENTED_EDGE('',*,*,#2140,.F.);
#2999=ORIENTED_EDGE('',*,*,#2141,.F.);
#3000=ORIENTED_EDGE('',*,*,#2131,.F.);
#3001=ORIENTED_EDGE('',*,*,#2138,.T.);
#3002=ORIENTED_EDGE('',*,*,#2142,.F.);
#3003=ORIENTED_EDGE('',*,*,#2143,.T.);
#3004=ORIENTED_EDGE('',*,*,#2144,.F.);
#3005=ORIENTED_EDGE('',*,*,#2135,.T.);
#3006=ORIENTED_EDGE('',*,*,#2144,.T.);
#3007=ORIENTED_EDGE('',*,*,#2145,.T.);
#3008=ORIENTED_EDGE('',*,*,#2146,.T.);
#3009=ORIENTED_EDGE('',*,*,#2147,.T.);
#3010=ORIENTED_EDGE('',*,*,#2148,.T.);
#3011=ORIENTED_EDGE('',*,*,#2149,.T.);
#3012=ORIENTED_EDGE('',*,*,#2150,.T.);
#3013=ORIENTED_EDGE('',*,*,#2151,.T.);
#3014=ORIENTED_EDGE('',*,*,#2139,.T.);
#3015=ORIENTED_EDGE('',*,*,#2130,.T.);
#3016=ORIENTED_EDGE('',*,*,#2122,.T.);
#3017=ORIENTED_EDGE('',*,*,#2129,.T.);
#3018=ORIENTED_EDGE('',*,*,#2127,.F.);
#3019=ORIENTED_EDGE('',*,*,#2134,.T.);
#3020=ORIENTED_EDGE('',*,*,#2152,.T.);
#3021=ORIENTED_EDGE('',*,*,#2153,.F.);
#3022=ORIENTED_EDGE('',*,*,#2154,.T.);
#3023=ORIENTED_EDGE('',*,*,#2145,.F.);
#3024=ORIENTED_EDGE('',*,*,#2143,.F.);
#3025=ORIENTED_EDGE('',*,*,#2155,.T.);
#3026=ORIENTED_EDGE('',*,*,#2156,.T.);
#3027=ORIENTED_EDGE('',*,*,#2147,.F.);
#3028=ORIENTED_EDGE('',*,*,#2157,.F.);
#3029=ORIENTED_EDGE('',*,*,#2158,.T.);
#3030=ORIENTED_EDGE('',*,*,#2159,.T.);
#3031=ORIENTED_EDGE('',*,*,#2160,.F.);
#3032=ORIENTED_EDGE('',*,*,#2161,.T.);
#3033=ORIENTED_EDGE('',*,*,#2162,.T.);
#3034=ORIENTED_EDGE('',*,*,#2157,.T.);
#3035=ORIENTED_EDGE('',*,*,#2146,.F.);
#3036=ORIENTED_EDGE('',*,*,#2154,.F.);
#3037=ORIENTED_EDGE('',*,*,#2163,.F.);
#3038=ORIENTED_EDGE('',*,*,#2164,.F.);
#3039=ORIENTED_EDGE('',*,*,#2165,.T.);
#3040=ORIENTED_EDGE('',*,*,#2166,.T.);
#3041=ORIENTED_EDGE('',*,*,#2167,.F.);
#3042=ORIENTED_EDGE('',*,*,#2159,.F.);
#3043=ORIENTED_EDGE('',*,*,#2168,.T.);
#3044=ORIENTED_EDGE('',*,*,#2165,.F.);
#3045=ORIENTED_EDGE('',*,*,#2169,.F.);
#3046=ORIENTED_EDGE('',*,*,#2162,.F.);
#3047=ORIENTED_EDGE('',*,*,#2170,.F.);
#3048=ORIENTED_EDGE('',*,*,#2166,.F.);
#3049=ORIENTED_EDGE('',*,*,#2168,.F.);
#3050=ORIENTED_EDGE('',*,*,#2158,.F.);
#3051=ORIENTED_EDGE('',*,*,#2161,.F.);
#3052=ORIENTED_EDGE('',*,*,#2171,.F.);
#3053=ORIENTED_EDGE('',*,*,#2167,.T.);
#3054=ORIENTED_EDGE('',*,*,#2170,.T.);
#3055=ORIENTED_EDGE('',*,*,#2140,.T.);
#3056=ORIENTED_EDGE('',*,*,#2151,.F.);
#3057=ORIENTED_EDGE('',*,*,#2172,.T.);
#3058=ORIENTED_EDGE('',*,*,#2173,.F.);
#3059=ORIENTED_EDGE('',*,*,#2149,.F.);
#3060=ORIENTED_EDGE('',*,*,#2174,.F.);
#3061=ORIENTED_EDGE('',*,*,#2175,.F.);
#3062=ORIENTED_EDGE('',*,*,#2176,.T.);
#3063=ORIENTED_EDGE('',*,*,#2148,.F.);
#3064=ORIENTED_EDGE('',*,*,#2156,.F.);
#3065=ORIENTED_EDGE('',*,*,#2177,.F.);
#3066=ORIENTED_EDGE('',*,*,#2174,.T.);
#3067=ORIENTED_EDGE('',*,*,#2150,.F.);
#3068=ORIENTED_EDGE('',*,*,#2176,.F.);
#3069=ORIENTED_EDGE('',*,*,#2178,.F.);
#3070=ORIENTED_EDGE('',*,*,#2172,.F.);
#3071=ORIENTED_EDGE('',*,*,#2179,.F.);
#3072=ORIENTED_EDGE('',*,*,#2180,.T.);
#3073=ORIENTED_EDGE('',*,*,#2155,.F.);
#3074=ORIENTED_EDGE('',*,*,#2180,.F.);
#3075=ORIENTED_EDGE('',*,*,#2136,.T.);
#3076=ORIENTED_EDGE('',*,*,#2152,.F.);
#3077=ORIENTED_EDGE('',*,*,#2133,.T.);
#3078=ORIENTED_EDGE('',*,*,#2181,.F.);
#3079=ORIENTED_EDGE('',*,*,#2179,.T.);
#3080=ORIENTED_EDGE('',*,*,#2137,.T.);
#3081=ORIENTED_EDGE('',*,*,#2181,.T.);
#3082=ORIENTED_EDGE('',*,*,#2132,.T.);
#3083=ORIENTED_EDGE('',*,*,#2141,.T.);
#3084=ORIENTED_EDGE('',*,*,#2173,.T.);
#3085=ORIENTED_EDGE('',*,*,#2178,.T.);
#3086=ORIENTED_EDGE('',*,*,#2175,.T.);
#3087=ORIENTED_EDGE('',*,*,#2177,.T.);
#3088=ORIENTED_EDGE('',*,*,#2160,.T.);
#3089=ORIENTED_EDGE('',*,*,#2169,.T.);
#3090=ORIENTED_EDGE('',*,*,#2164,.T.);
#3091=ORIENTED_EDGE('',*,*,#2171,.T.);
#3092=ORIENTED_EDGE('',*,*,#2163,.T.);
#3093=ORIENTED_EDGE('',*,*,#2153,.T.);
#3094=ORIENTED_EDGE('',*,*,#2142,.T.);
#3095=ORIENTED_EDGE('',*,*,#2182,.T.);
#3096=ORIENTED_EDGE('',*,*,#2183,.T.);
#3097=ORIENTED_EDGE('',*,*,#2184,.F.);
#3098=ORIENTED_EDGE('',*,*,#2183,.F.);
#3099=ORIENTED_EDGE('',*,*,#2184,.T.);
#3100=ORIENTED_EDGE('',*,*,#2182,.F.);
#3101=ORIENTED_EDGE('',*,*,#2185,.F.);
#3102=ORIENTED_EDGE('',*,*,#2186,.T.);
#3103=ORIENTED_EDGE('',*,*,#2187,.T.);
#3104=ORIENTED_EDGE('',*,*,#2188,.F.);
#3105=ORIENTED_EDGE('',*,*,#2189,.F.);
#3106=ORIENTED_EDGE('',*,*,#2190,.T.);
#3107=ORIENTED_EDGE('',*,*,#2191,.T.);
#3108=ORIENTED_EDGE('',*,*,#2186,.F.);
#3109=ORIENTED_EDGE('',*,*,#2192,.F.);
#3110=ORIENTED_EDGE('',*,*,#2193,.T.);
#3111=ORIENTED_EDGE('',*,*,#2194,.T.);
#3112=ORIENTED_EDGE('',*,*,#2190,.F.);
#3113=ORIENTED_EDGE('',*,*,#2195,.F.);
#3114=ORIENTED_EDGE('',*,*,#2188,.T.);
#3115=ORIENTED_EDGE('',*,*,#2196,.T.);
#3116=ORIENTED_EDGE('',*,*,#2193,.F.);
#3117=ORIENTED_EDGE('',*,*,#2197,.F.);
#3118=ORIENTED_EDGE('',*,*,#2198,.F.);
#3119=ORIENTED_EDGE('',*,*,#2199,.F.);
#3120=ORIENTED_EDGE('',*,*,#2200,.F.);
#3121=ORIENTED_EDGE('',*,*,#2196,.F.);
#3122=ORIENTED_EDGE('',*,*,#2187,.F.);
#3123=ORIENTED_EDGE('',*,*,#2191,.F.);
#3124=ORIENTED_EDGE('',*,*,#2194,.F.);
#3125=ORIENTED_EDGE('',*,*,#2198,.T.);
#3126=ORIENTED_EDGE('',*,*,#2201,.T.);
#3127=ORIENTED_EDGE('',*,*,#2202,.F.);
#3128=ORIENTED_EDGE('',*,*,#2203,.F.);
#3129=ORIENTED_EDGE('',*,*,#2197,.T.);
#3130=ORIENTED_EDGE('',*,*,#2204,.T.);
#3131=ORIENTED_EDGE('',*,*,#2205,.F.);
#3132=ORIENTED_EDGE('',*,*,#2201,.F.);
#3133=ORIENTED_EDGE('',*,*,#2206,.F.);
#3134=ORIENTED_EDGE('',*,*,#2207,.T.);
#3135=ORIENTED_EDGE('',*,*,#2208,.T.);
#3136=ORIENTED_EDGE('',*,*,#2209,.F.);
#3137=ORIENTED_EDGE('',*,*,#2210,.F.);
#3138=ORIENTED_EDGE('',*,*,#2211,.T.);
#3139=ORIENTED_EDGE('',*,*,#2212,.T.);
#3140=ORIENTED_EDGE('',*,*,#2207,.F.);
#3141=ORIENTED_EDGE('',*,*,#2213,.F.);
#3142=ORIENTED_EDGE('',*,*,#2214,.T.);
#3143=ORIENTED_EDGE('',*,*,#2215,.T.);
#3144=ORIENTED_EDGE('',*,*,#2211,.F.);
#3145=ORIENTED_EDGE('',*,*,#2216,.F.);
#3146=ORIENTED_EDGE('',*,*,#2209,.T.);
#3147=ORIENTED_EDGE('',*,*,#2217,.T.);
#3148=ORIENTED_EDGE('',*,*,#2214,.F.);
#3149=ORIENTED_EDGE('',*,*,#2217,.F.);
#3150=ORIENTED_EDGE('',*,*,#2208,.F.);
#3151=ORIENTED_EDGE('',*,*,#2212,.F.);
#3152=ORIENTED_EDGE('',*,*,#2215,.F.);
#3153=ORIENTED_EDGE('',*,*,#2199,.T.);
#3154=ORIENTED_EDGE('',*,*,#2203,.T.);
#3155=ORIENTED_EDGE('',*,*,#2218,.F.);
#3156=ORIENTED_EDGE('',*,*,#2219,.F.);
#3157=ORIENTED_EDGE('',*,*,#2200,.T.);
#3158=ORIENTED_EDGE('',*,*,#2219,.T.);
#3159=ORIENTED_EDGE('',*,*,#2220,.F.);
#3160=ORIENTED_EDGE('',*,*,#2204,.F.);
#3161=ORIENTED_EDGE('',*,*,#2185,.T.);
#3162=ORIENTED_EDGE('',*,*,#2195,.T.);
#3163=ORIENTED_EDGE('',*,*,#2192,.T.);
#3164=ORIENTED_EDGE('',*,*,#2189,.T.);
#3165=ORIENTED_EDGE('',*,*,#2206,.T.);
#3166=ORIENTED_EDGE('',*,*,#2216,.T.);
#3167=ORIENTED_EDGE('',*,*,#2213,.T.);
#3168=ORIENTED_EDGE('',*,*,#2210,.T.);
#3169=ORIENTED_EDGE('',*,*,#2202,.T.);
#3170=ORIENTED_EDGE('',*,*,#2205,.T.);
#3171=ORIENTED_EDGE('',*,*,#2220,.T.);
#3172=ORIENTED_EDGE('',*,*,#2218,.T.);
#3173=CYLINDRICAL_SURFACE('',#3520,0.946);
#3174=CYLINDRICAL_SURFACE('',#3531,0.946);
#3175=CYLINDRICAL_SURFACE('',#3541,0.946);
#3176=CYLINDRICAL_SURFACE('',#3547,0.946);
#3177=CYLINDRICAL_SURFACE('',#3568,2.17846096908266);
#3178=CYLINDRICAL_SURFACE('',#3572,2.4505);
#3179=CYLINDRICAL_SURFACE('',#3581,0.946);
#3180=CYLINDRICAL_SURFACE('',#3592,0.946);
#3181=CYLINDRICAL_SURFACE('',#3602,0.946);
#3182=CYLINDRICAL_SURFACE('',#3608,0.946);
#3183=CYLINDRICAL_SURFACE('',#3629,2.17846096908266);
#3184=CYLINDRICAL_SURFACE('',#3633,2.4505);
#3185=CYLINDRICAL_SURFACE('',#3642,0.946);
#3186=CYLINDRICAL_SURFACE('',#3653,0.946);
#3187=CYLINDRICAL_SURFACE('',#3663,0.946);
#3188=CYLINDRICAL_SURFACE('',#3669,0.946);
#3189=CYLINDRICAL_SURFACE('',#3690,2.17846096908266);
#3190=CYLINDRICAL_SURFACE('',#3694,2.4505);
#3191=CYLINDRICAL_SURFACE('',#3703,0.946);
#3192=CYLINDRICAL_SURFACE('',#3714,0.946);
#3193=CYLINDRICAL_SURFACE('',#3724,0.946);
#3194=CYLINDRICAL_SURFACE('',#3730,0.946);
#3195=CYLINDRICAL_SURFACE('',#3751,2.17846096908266);
#3196=CYLINDRICAL_SURFACE('',#3755,2.4505);
#3197=CYLINDRICAL_SURFACE('',#3777,2.5175);
#3198=CYLINDRICAL_SURFACE('',#3778,2.5175);
#3199=CYLINDRICAL_SURFACE('',#3786,2.5);
#3200=CYLINDRICAL_SURFACE('',#3799,4.99999999999999);
#3201=CYLINDRICAL_SURFACE('',#3807,4.99999999999999);
#3202=CYLINDRICAL_SURFACE('',#3824,2.5175);
#3203=CYLINDRICAL_SURFACE('',#3825,2.5175);
#3204=CYLINDRICAL_SURFACE('',#3835,4.99999999999999);
#3205=CYLINDRICAL_SURFACE('',#3844,4.99999999999999);
#3206=CYLINDRICAL_SURFACE('',#3851,4.99999999999999);
#3207=CYLINDRICAL_SURFACE('',#3856,2.5);
#3208=ADVANCED_FACE('',(#266),#3173,.T.);
#3209=ADVANCED_FACE('',(#267),#129,.F.);
#3210=ADVANCED_FACE('',(#268),#130,.F.);
#3211=ADVANCED_FACE('',(#269),#131,.F.);
#3212=ADVANCED_FACE('',(#270),#3174,.T.);
#3213=ADVANCED_FACE('',(#271),#132,.F.);
#3214=ADVANCED_FACE('',(#272),#133,.F.);
#3215=ADVANCED_FACE('',(#273),#134,.F.);
#3216=ADVANCED_FACE('',(#274),#3175,.T.);
#3217=ADVANCED_FACE('',(#275),#135,.F.);
#3218=ADVANCED_FACE('',(#276),#3176,.T.);
#3219=ADVANCED_FACE('',(#277),#136,.F.);
#3220=ADVANCED_FACE('',(#278),#137,.F.);
#3221=ADVANCED_FACE('',(#279),#138,.F.);
#3222=ADVANCED_FACE('',(#280),#139,.F.);
#3223=ADVANCED_FACE('',(#281),#140,.F.);
#3224=ADVANCED_FACE('',(#282),#141,.F.);
#3225=ADVANCED_FACE('',(#283),#125,.F.);
#3226=ADVANCED_FACE('',(#284,#107),#142,.T.);
#3227=ADVANCED_FACE('',(#285),#3177,.T.);
#3228=ADVANCED_FACE('',(#286),#99,.T.);
#3229=ADVANCED_FACE('',(#287),#3178,.T.);
#3230=ADVANCED_FACE('',(#288),#143,.T.);
#3231=ADVANCED_FACE('',(#289),#95,.T.);
#3232=ADVANCED_FACE('',(#290),#100,.T.);
#3233=ADVANCED_FACE('',(#291),#3179,.T.);
#3234=ADVANCED_FACE('',(#292),#144,.F.);
#3235=ADVANCED_FACE('',(#293),#145,.F.);
#3236=ADVANCED_FACE('',(#294),#146,.F.);
#3237=ADVANCED_FACE('',(#295),#3180,.T.);
#3238=ADVANCED_FACE('',(#296),#147,.F.);
#3239=ADVANCED_FACE('',(#297),#148,.F.);
#3240=ADVANCED_FACE('',(#298),#149,.F.);
#3241=ADVANCED_FACE('',(#299),#3181,.T.);
#3242=ADVANCED_FACE('',(#300),#150,.F.);
#3243=ADVANCED_FACE('',(#301),#3182,.T.);
#3244=ADVANCED_FACE('',(#302),#151,.F.);
#3245=ADVANCED_FACE('',(#303),#152,.F.);
#3246=ADVANCED_FACE('',(#304),#153,.F.);
#3247=ADVANCED_FACE('',(#305),#154,.F.);
#3248=ADVANCED_FACE('',(#306),#155,.F.);
#3249=ADVANCED_FACE('',(#307),#156,.F.);
#3250=ADVANCED_FACE('',(#308),#126,.F.);
#3251=ADVANCED_FACE('',(#309,#108),#157,.T.);
#3252=ADVANCED_FACE('',(#310),#3183,.T.);
#3253=ADVANCED_FACE('',(#311),#101,.T.);
#3254=ADVANCED_FACE('',(#312),#3184,.T.);
#3255=ADVANCED_FACE('',(#313),#158,.T.);
#3256=ADVANCED_FACE('',(#314),#96,.T.);
#3257=ADVANCED_FACE('',(#315),#102,.T.);
#3258=ADVANCED_FACE('',(#316),#3185,.T.);
#3259=ADVANCED_FACE('',(#317),#159,.F.);
#3260=ADVANCED_FACE('',(#318),#160,.F.);
#3261=ADVANCED_FACE('',(#319),#161,.F.);
#3262=ADVANCED_FACE('',(#320),#3186,.T.);
#3263=ADVANCED_FACE('',(#321),#162,.F.);
#3264=ADVANCED_FACE('',(#322),#163,.F.);
#3265=ADVANCED_FACE('',(#323),#164,.F.);
#3266=ADVANCED_FACE('',(#324),#3187,.T.);
#3267=ADVANCED_FACE('',(#325),#165,.F.);
#3268=ADVANCED_FACE('',(#326),#3188,.T.);
#3269=ADVANCED_FACE('',(#327),#166,.F.);
#3270=ADVANCED_FACE('',(#328),#167,.F.);
#3271=ADVANCED_FACE('',(#329),#168,.F.);
#3272=ADVANCED_FACE('',(#330),#169,.F.);
#3273=ADVANCED_FACE('',(#331),#170,.F.);
#3274=ADVANCED_FACE('',(#332),#171,.F.);
#3275=ADVANCED_FACE('',(#333),#127,.F.);
#3276=ADVANCED_FACE('',(#334,#109),#172,.T.);
#3277=ADVANCED_FACE('',(#335),#3189,.T.);
#3278=ADVANCED_FACE('',(#336),#103,.T.);
#3279=ADVANCED_FACE('',(#337),#3190,.T.);
#3280=ADVANCED_FACE('',(#338),#173,.T.);
#3281=ADVANCED_FACE('',(#339),#97,.T.);
#3282=ADVANCED_FACE('',(#340),#104,.T.);
#3283=ADVANCED_FACE('',(#341),#3191,.T.);
#3284=ADVANCED_FACE('',(#342),#174,.F.);
#3285=ADVANCED_FACE('',(#343),#175,.F.);
#3286=ADVANCED_FACE('',(#344),#176,.F.);
#3287=ADVANCED_FACE('',(#345),#3192,.T.);
#3288=ADVANCED_FACE('',(#346),#177,.F.);
#3289=ADVANCED_FACE('',(#347),#178,.F.);
#3290=ADVANCED_FACE('',(#348),#179,.F.);
#3291=ADVANCED_FACE('',(#349),#3193,.T.);
#3292=ADVANCED_FACE('',(#350),#180,.F.);
#3293=ADVANCED_FACE('',(#351),#3194,.T.);
#3294=ADVANCED_FACE('',(#352),#181,.F.);
#3295=ADVANCED_FACE('',(#353),#182,.F.);
#3296=ADVANCED_FACE('',(#354),#183,.F.);
#3297=ADVANCED_FACE('',(#355),#184,.F.);
#3298=ADVANCED_FACE('',(#356),#185,.F.);
#3299=ADVANCED_FACE('',(#357),#186,.F.);
#3300=ADVANCED_FACE('',(#358),#128,.F.);
#3301=ADVANCED_FACE('',(#359,#110),#187,.T.);
#3302=ADVANCED_FACE('',(#360),#3195,.T.);
#3303=ADVANCED_FACE('',(#361),#105,.T.);
#3304=ADVANCED_FACE('',(#362),#3196,.T.);
#3305=ADVANCED_FACE('',(#363),#188,.T.);
#3306=ADVANCED_FACE('',(#364),#98,.T.);
#3307=ADVANCED_FACE('',(#365),#106,.T.);
#3308=ADVANCED_FACE('',(#366),#189,.T.);
#3309=ADVANCED_FACE('',(#367),#190,.T.);
#3310=ADVANCED_FACE('',(#368),#191,.T.);
#3311=ADVANCED_FACE('',(#369),#192,.T.);
#3312=ADVANCED_FACE('',(#370,#111,#112),#193,.F.);
#3313=ADVANCED_FACE('',(#371),#194,.F.);
#3314=ADVANCED_FACE('',(#372,#113,#114),#195,.T.);
#3315=ADVANCED_FACE('',(#373),#196,.T.);
#3316=ADVANCED_FACE('',(#374),#197,.T.);
#3317=ADVANCED_FACE('',(#375),#3197,.F.);
#3318=ADVANCED_FACE('',(#376),#3198,.F.);
#3319=ADVANCED_FACE('',(#377),#198,.T.);
#3320=ADVANCED_FACE('',(#378),#199,.T.);
#3321=ADVANCED_FACE('',(#379),#200,.T.);
#3322=ADVANCED_FACE('',(#380),#201,.T.);
#3323=ADVANCED_FACE('',(#381),#202,.T.);
#3324=ADVANCED_FACE('',(#382),#203,.F.);
#3325=ADVANCED_FACE('',(#383),#3199,.F.);
#3326=ADVANCED_FACE('',(#384),#204,.F.);
#3327=ADVANCED_FACE('',(#385),#205,.F.);
#3328=ADVANCED_FACE('',(#386),#206,.F.);
#3329=ADVANCED_FACE('',(#387),#207,.F.);
#3330=ADVANCED_FACE('',(#388),#208,.F.);
#3331=ADVANCED_FACE('',(#389),#209,.F.);
#3332=ADVANCED_FACE('',(#390),#210,.F.);
#3333=ADVANCED_FACE('',(#391),#211,.F.);
#3334=ADVANCED_FACE('',(#392,#115),#212,.F.);
#3335=ADVANCED_FACE('',(#393),#3200,.F.);
#3336=ADVANCED_FACE('',(#394,#116),#213,.T.);
#3337=ADVANCED_FACE('',(#395),#214,.F.);
#3338=ADVANCED_FACE('',(#396),#215,.F.);
#3339=ADVANCED_FACE('',(#397),#216,.T.);
#3340=ADVANCED_FACE('',(#398),#3201,.F.);
#3341=ADVANCED_FACE('',(#399),#217,.T.);
#3342=ADVANCED_FACE('',(#400),#218,.F.);
#3343=ADVANCED_FACE('',(#401),#219,.F.);
#3344=ADVANCED_FACE('',(#402),#220,.F.);
#3345=ADVANCED_FACE('',(#403),#221,.F.);
#3346=ADVANCED_FACE('',(#404),#222,.F.);
#3347=ADVANCED_FACE('',(#405),#223,.F.);
#3348=ADVANCED_FACE('',(#406,#117,#118),#224,.T.);
#3349=ADVANCED_FACE('',(#407),#225,.T.);
#3350=ADVANCED_FACE('',(#408,#119,#120),#226,.F.);
#3351=ADVANCED_FACE('',(#409),#227,.T.);
#3352=ADVANCED_FACE('',(#410),#3202,.F.);
#3353=ADVANCED_FACE('',(#411),#3203,.F.);
#3354=ADVANCED_FACE('',(#412),#228,.T.);
#3355=ADVANCED_FACE('',(#413),#229,.F.);
#3356=ADVANCED_FACE('',(#414),#230,.F.);
#3357=ADVANCED_FACE('',(#415),#231,.F.);
#3358=ADVANCED_FACE('',(#416),#232,.F.);
#3359=ADVANCED_FACE('',(#417),#233,.F.);
#3360=ADVANCED_FACE('',(#418),#234,.F.);
#3361=ADVANCED_FACE('',(#419),#235,.F.);
#3362=ADVANCED_FACE('',(#420),#3204,.F.);
#3363=ADVANCED_FACE('',(#421),#236,.F.);
#3364=ADVANCED_FACE('',(#422,#121),#237,.F.);
#3365=ADVANCED_FACE('',(#423),#238,.F.);
#3366=ADVANCED_FACE('',(#424),#3205,.F.);
#3367=ADVANCED_FACE('',(#425),#239,.F.);
#3368=ADVANCED_FACE('',(#426),#240,.F.);
#3369=ADVANCED_FACE('',(#427),#241,.F.);
#3370=ADVANCED_FACE('',(#428),#242,.F.);
#3371=ADVANCED_FACE('',(#429),#3206,.F.);
#3372=ADVANCED_FACE('',(#430),#243,.F.);
#3373=ADVANCED_FACE('',(#431),#244,.F.);
#3374=ADVANCED_FACE('',(#432),#245,.F.);
#3375=ADVANCED_FACE('',(#433),#3207,.F.);
#3376=ADVANCED_FACE('',(#434,#122),#246,.T.);
#3377=ADVANCED_FACE('',(#435),#247,.T.);
#3378=ADVANCED_FACE('',(#436),#51,.T.);
#3379=ADVANCED_FACE('',(#437),#248,.T.);
#3380=ADVANCED_FACE('',(#438),#249,.F.);
#3381=ADVANCED_FACE('',(#439),#250,.F.);
#3382=ADVANCED_FACE('',(#440),#251,.F.);
#3383=ADVANCED_FACE('',(#441),#252,.F.);
#3384=ADVANCED_FACE('',(#442),#253,.F.);
#3385=ADVANCED_FACE('',(#443,#123),#254,.F.);
#3386=ADVANCED_FACE('',(#444),#255,.T.);
#3387=ADVANCED_FACE('',(#445),#256,.T.);
#3388=ADVANCED_FACE('',(#446),#257,.F.);
#3389=ADVANCED_FACE('',(#447),#258,.F.);
#3390=ADVANCED_FACE('',(#448),#259,.F.);
#3391=ADVANCED_FACE('',(#449),#260,.F.);
#3392=ADVANCED_FACE('',(#450),#261,.F.);
#3393=ADVANCED_FACE('',(#451),#262,.T.);
#3394=ADVANCED_FACE('',(#452),#263,.T.);
#3395=ADVANCED_FACE('',(#453,#124),#264,.T.);
#3396=ADVANCED_FACE('',(#454),#265,.T.);
#3397=CLOSED_SHELL('',(#3208,#3209,#3210,#3211,#3212,#3213,#3214,#3215,
#3216,#3217,#3218,#3219,#3220,#3221,#3222,#3223,#3224,#3225,#3226,#3227,
#3228,#3229,#3230,#3231,#3232));
#3398=CLOSED_SHELL('',(#3233,#3234,#3235,#3236,#3237,#3238,#3239,#3240,
#3241,#3242,#3243,#3244,#3245,#3246,#3247,#3248,#3249,#3250,#3251,#3252,
#3253,#3254,#3255,#3256,#3257));
#3399=CLOSED_SHELL('',(#3258,#3259,#3260,#3261,#3262,#3263,#3264,#3265,
#3266,#3267,#3268,#3269,#3270,#3271,#3272,#3273,#3274,#3275,#3276,#3277,
#3278,#3279,#3280,#3281,#3282));
#3400=CLOSED_SHELL('',(#3283,#3284,#3285,#3286,#3287,#3288,#3289,#3290,
#3291,#3292,#3293,#3294,#3295,#3296,#3297,#3298,#3299,#3300,#3301,#3302,
#3303,#3304,#3305,#3306,#3307));
#3401=CLOSED_SHELL('',(#3308,#3309,#3310,#3311,#3312,#3313,#3314,#3315,
#3316,#3317,#3318,#3319));
#3402=CLOSED_SHELL('',(#3320,#3321,#3322,#3323,#3324,#3325,#3326,#3327,
#3328,#3329,#3330,#3331,#3332,#3333,#3334,#3335,#3336,#3337,#3338,#3339,
#3340,#3341,#3342));
#3403=CLOSED_SHELL('',(#3343,#3344,#3345,#3346,#3347,#3348,#3349,#3350,
#3351,#3352,#3353,#3354));
#3404=CLOSED_SHELL('',(#3355,#3356,#3357,#3358,#3359,#3360,#3361,#3362,
#3363,#3364,#3365,#3366,#3367,#3368,#3369,#3370,#3371,#3372,#3373,#3374,
#3375,#3376,#3377));
#3405=CLOSED_SHELL('',(#3378,#3379,#3380));
#3406=CLOSED_SHELL('',(#3381,#3382,#3383,#3384,#3385,#3386,#3387,#3388,
#3389,#3390,#3391,#3392,#3393,#3394,#3395,#3396));
#3407=DERIVED_UNIT_ELEMENT(#3427,1.);
#3408=DERIVED_UNIT_ELEMENT(#7049,-3.);
#3409=DERIVED_UNIT_ELEMENT(#3427,1.);
#3410=DERIVED_UNIT_ELEMENT(#7049,-3.);
#3411=DERIVED_UNIT_ELEMENT(#3427,1.);
#3412=DERIVED_UNIT_ELEMENT(#7049,-3.);
#3413=DERIVED_UNIT_ELEMENT(#3427,1.);
#3414=DERIVED_UNIT_ELEMENT(#7049,-3.);
#3415=DERIVED_UNIT_ELEMENT(#3427,1.);
#3416=DERIVED_UNIT_ELEMENT(#7049,-3.);
#3417=DERIVED_UNIT_ELEMENT(#3427,1.);
#3418=DERIVED_UNIT_ELEMENT(#7049,-3.);
#3419=DERIVED_UNIT_ELEMENT(#3427,1.);
#3420=DERIVED_UNIT_ELEMENT(#7049,-3.);
#3421=DERIVED_UNIT_ELEMENT(#3427,1.);
#3422=DERIVED_UNIT_ELEMENT(#7049,-3.);
#3423=DERIVED_UNIT_ELEMENT(#3427,1.);
#3424=DERIVED_UNIT_ELEMENT(#7049,-3.);
#3425=DERIVED_UNIT_ELEMENT(#3427,1.);
#3426=DERIVED_UNIT_ELEMENT(#7049,-3.);
#3427=(
MASS_UNIT()
NAMED_UNIT(*)
SI_UNIT(.KILO.,.GRAM.)
);
#3428=DERIVED_UNIT((#3407,#3408));
#3429=DERIVED_UNIT((#3409,#3410));
#3430=DERIVED_UNIT((#3411,#3412));
#3431=DERIVED_UNIT((#3413,#3414));
#3432=DERIVED_UNIT((#3415,#3416));
#3433=DERIVED_UNIT((#3417,#3418));
#3434=DERIVED_UNIT((#3419,#3420));
#3435=DERIVED_UNIT((#3421,#3422));
#3436=DERIVED_UNIT((#3423,#3424));
#3437=DERIVED_UNIT((#3425,#3426));
#3438=MEASURE_REPRESENTATION_ITEM('density measure',
POSITIVE_RATIO_MEASURE(7750.),#3428);
#3439=MEASURE_REPRESENTATION_ITEM('density measure',
POSITIVE_RATIO_MEASURE(7750.),#3429);
#3440=MEASURE_REPRESENTATION_ITEM('density measure',
POSITIVE_RATIO_MEASURE(7750.),#3430);
#3441=MEASURE_REPRESENTATION_ITEM('density measure',
POSITIVE_RATIO_MEASURE(7750.),#3431);
#3442=MEASURE_REPRESENTATION_ITEM('density measure',
POSITIVE_RATIO_MEASURE(7850.),#3432);
#3443=MEASURE_REPRESENTATION_ITEM('density measure',
POSITIVE_RATIO_MEASURE(7850.),#3433);
#3444=MEASURE_REPRESENTATION_ITEM('density measure',
POSITIVE_RATIO_MEASURE(7850.),#3434);
#3445=MEASURE_REPRESENTATION_ITEM('density measure',
POSITIVE_RATIO_MEASURE(7850.),#3435);
#3446=MEASURE_REPRESENTATION_ITEM('density measure',
POSITIVE_RATIO_MEASURE(7850.),#3436);
#3447=MEASURE_REPRESENTATION_ITEM('density measure',
POSITIVE_RATIO_MEASURE(7850.),#3437);
#3448=PROPERTY_DEFINITION_REPRESENTATION(#3498,#3468);
#3449=PROPERTY_DEFINITION_REPRESENTATION(#3499,#3469);
#3450=PROPERTY_DEFINITION_REPRESENTATION(#3500,#3470);
#3451=PROPERTY_DEFINITION_REPRESENTATION(#3501,#3471);
#3452=PROPERTY_DEFINITION_REPRESENTATION(#3502,#3472);
#3453=PROPERTY_DEFINITION_REPRESENTATION(#3503,#3473);
#3454=PROPERTY_DEFINITION_REPRESENTATION(#3504,#3474);
#3455=PROPERTY_DEFINITION_REPRESENTATION(#3505,#3475);
#3456=PROPERTY_DEFINITION_REPRESENTATION(#3506,#3476);
#3457=PROPERTY_DEFINITION_REPRESENTATION(#3507,#3477);
#3458=PROPERTY_DEFINITION_REPRESENTATION(#3508,#3478);
#3459=PROPERTY_DEFINITION_REPRESENTATION(#3509,#3479);
#3460=PROPERTY_DEFINITION_REPRESENTATION(#3510,#3480);
#3461=PROPERTY_DEFINITION_REPRESENTATION(#3511,#3481);
#3462=PROPERTY_DEFINITION_REPRESENTATION(#3512,#3482);
#3463=PROPERTY_DEFINITION_REPRESENTATION(#3513,#3483);
#3464=PROPERTY_DEFINITION_REPRESENTATION(#3514,#3484);
#3465=PROPERTY_DEFINITION_REPRESENTATION(#3515,#3485);
#3466=PROPERTY_DEFINITION_REPRESENTATION(#3516,#3486);
#3467=PROPERTY_DEFINITION_REPRESENTATION(#3517,#3487);
#3468=REPRESENTATION('material name',(#3488),#7037);
#3469=REPRESENTATION('density',(#3438),#7037);
#3470=REPRESENTATION('material name',(#3489),#7038);
#3471=REPRESENTATION('density',(#3439),#7038);
#3472=REPRESENTATION('material name',(#3490),#7039);
#3473=REPRESENTATION('density',(#3440),#7039);
#3474=REPRESENTATION('material name',(#3491),#7040);
#3475=REPRESENTATION('density',(#3441),#7040);
#3476=REPRESENTATION('material name',(#3492),#7041);
#3477=REPRESENTATION('density',(#3442),#7041);
#3478=REPRESENTATION('material name',(#3493),#7042);
#3479=REPRESENTATION('density',(#3443),#7042);
#3480=REPRESENTATION('material name',(#3494),#7043);
#3481=REPRESENTATION('density',(#3444),#7043);
#3482=REPRESENTATION('material name',(#3495),#7044);
#3483=REPRESENTATION('density',(#3445),#7044);
#3484=REPRESENTATION('material name',(#3496),#7045);
#3485=REPRESENTATION('density',(#3446),#7045);
#3486=REPRESENTATION('material name',(#3497),#7046);
#3487=REPRESENTATION('density',(#3447),#7046);
#3488=DESCRIPTIVE_REPRESENTATION_ITEM('Steel 4.6, Plain',
'Steel 4.6, Plain');
#3489=DESCRIPTIVE_REPRESENTATION_ITEM('Steel 4.6, Plain',
'Steel 4.6, Plain');
#3490=DESCRIPTIVE_REPRESENTATION_ITEM('Steel 4.6, Plain',
'Steel 4.6, Plain');
#3491=DESCRIPTIVE_REPRESENTATION_ITEM('Steel 4.6, Plain',
'Steel 4.6, Plain');
#3492=DESCRIPTIVE_REPRESENTATION_ITEM('Steel','Steel');
#3493=DESCRIPTIVE_REPRESENTATION_ITEM('Steel','Steel');
#3494=DESCRIPTIVE_REPRESENTATION_ITEM('Steel','Steel');
#3495=DESCRIPTIVE_REPRESENTATION_ITEM('Steel','Steel');
#3496=DESCRIPTIVE_REPRESENTATION_ITEM('Steel','Steel');
#3497=DESCRIPTIVE_REPRESENTATION_ITEM('Steel','Steel');
#3498=PROPERTY_DEFINITION('material property','material name',#7097);
#3499=PROPERTY_DEFINITION('material property','density of part',#7097);
#3500=PROPERTY_DEFINITION('material property','material name',#7098);
#3501=PROPERTY_DEFINITION('material property','density of part',#7098);
#3502=PROPERTY_DEFINITION('material property','material name',#7099);
#3503=PROPERTY_DEFINITION('material property','density of part',#7099);
#3504=PROPERTY_DEFINITION('material property','material name',#7100);
#3505=PROPERTY_DEFINITION('material property','density of part',#7100);
#3506=PROPERTY_DEFINITION('material property','material name',#7101);
#3507=PROPERTY_DEFINITION('material property','density of part',#7101);
#3508=PROPERTY_DEFINITION('material property','material name',#7102);
#3509=PROPERTY_DEFINITION('material property','density of part',#7102);
#3510=PROPERTY_DEFINITION('material property','material name',#7103);
#3511=PROPERTY_DEFINITION('material property','density of part',#7103);
#3512=PROPERTY_DEFINITION('material property','material name',#7104);
#3513=PROPERTY_DEFINITION('material property','density of part',#7104);
#3514=PROPERTY_DEFINITION('material property','material name',#7105);
#3515=PROPERTY_DEFINITION('material property','density of part',#7105);
#3516=PROPERTY_DEFINITION('material property','material name',#7106);
#3517=PROPERTY_DEFINITION('material property','density of part',#7106);
#3518=AXIS2_PLACEMENT_3D('',#4934,#3892,#3893);
#3519=AXIS2_PLACEMENT_3D('',#4935,#3894,#3895);
#3520=AXIS2_PLACEMENT_3D('',#4936,#3896,#3897);
#3521=AXIS2_PLACEMENT_3D('',#4957,#3899,#3900);
#3522=AXIS2_PLACEMENT_3D('',#4959,#3901,#3902);
#3523=AXIS2_PLACEMENT_3D('',#4961,#3903,#3904);
#3524=AXIS2_PLACEMENT_3D('',#4963,#3906,#3907);
#3525=AXIS2_PLACEMENT_3D('',#4965,#3908,#3909);
#3526=AXIS2_PLACEMENT_3D('',#4967,#3911,#3912);
#3527=AXIS2_PLACEMENT_3D('',#4969,#3913,#3914);
#3528=AXIS2_PLACEMENT_3D('',#4973,#3916,#3917);
#3529=AXIS2_PLACEMENT_3D('',#4975,#3919,#3920);
#3530=AXIS2_PLACEMENT_3D('',#4977,#3921,#3922);
#3531=AXIS2_PLACEMENT_3D('',#4979,#3924,#3925);
#3532=AXIS2_PLACEMENT_3D('',#4997,#3926,#3927);
#3533=AXIS2_PLACEMENT_3D('',#4999,#3928,#3929);
#3534=AXIS2_PLACEMENT_3D('',#5001,#3931,#3932);
#3535=AXIS2_PLACEMENT_3D('',#5003,#3933,#3934);
#3536=AXIS2_PLACEMENT_3D('',#5005,#3936,#3937);
#3537=AXIS2_PLACEMENT_3D('',#5007,#3938,#3939);
#3538=AXIS2_PLACEMENT_3D('',#5011,#3941,#3942);
#3539=AXIS2_PLACEMENT_3D('',#5013,#3944,#3945);
#3540=AXIS2_PLACEMENT_3D('',#5015,#3946,#3947);
#3541=AXIS2_PLACEMENT_3D('',#5017,#3949,#3950);
#3542=AXIS2_PLACEMENT_3D('',#5038,#3952,#3953);
#3543=AXIS2_PLACEMENT_3D('',#5040,#3954,#3955);
#3544=AXIS2_PLACEMENT_3D('',#5042,#3956,#3957);
#3545=AXIS2_PLACEMENT_3D('',#5044,#3959,#3960);
#3546=AXIS2_PLACEMENT_3D('',#5046,#3961,#3962);
#3547=AXIS2_PLACEMENT_3D('',#5048,#3964,#3965);
#3548=AXIS2_PLACEMENT_3D('',#5066,#3966,#3967);
#3549=AXIS2_PLACEMENT_3D('',#5068,#3968,#3969);
#3550=AXIS2_PLACEMENT_3D('',#5070,#3971,#3972);
#3551=AXIS2_PLACEMENT_3D('',#5072,#3973,#3974);
#3552=AXIS2_PLACEMENT_3D('',#5074,#3976,#3977);
#3553=AXIS2_PLACEMENT_3D('',#5076,#3978,#3979);
#3554=AXIS2_PLACEMENT_3D('',#5078,#3981,#3982);
#3555=AXIS2_PLACEMENT_3D('',#5080,#3983,#3984);
#3556=AXIS2_PLACEMENT_3D('',#5082,#3986,#3987);
#3557=AXIS2_PLACEMENT_3D('',#5083,#3988,#3989);
#3558=AXIS2_PLACEMENT_3D('',#5085,#3990,#3991);
#3559=AXIS2_PLACEMENT_3D('',#5087,#3993,#3994);
#3560=AXIS2_PLACEMENT_3D('',#5088,#3995,#3996);
#3561=AXIS2_PLACEMENT_3D('',#5090,#3998,#3999);
#3562=AXIS2_PLACEMENT_3D('',#5091,#4000,#4001);
#3563=AXIS2_PLACEMENT_3D('',#5093,#4002,#4003);
#3564=AXIS2_PLACEMENT_3D('',#5095,#4004,#4005);
#3565=AXIS2_PLACEMENT_3D('',#5096,#4006,#4007);
#3566=AXIS2_PLACEMENT_3D('',#5097,#4008,#4009);
#3567=AXIS2_PLACEMENT_3D('',#5099,#4010,#4011);
#3568=AXIS2_PLACEMENT_3D('',#5100,#4012,#4013);
#3569=AXIS2_PLACEMENT_3D('',#5102,#4014,#4015);
#3570=AXIS2_PLACEMENT_3D('',#5104,#4017,#4018);
#3571=AXIS2_PLACEMENT_3D('',#5106,#4019,#4020);
#3572=AXIS2_PLACEMENT_3D('',#5108,#4022,#4023);
#3573=AXIS2_PLACEMENT_3D('',#5110,#4024,#4025);
#3574=AXIS2_PLACEMENT_3D('',#5112,#4027,#4028);
#3575=AXIS2_PLACEMENT_3D('',#5113,#4029,#4030);
#3576=AXIS2_PLACEMENT_3D('',#5115,#4031,#4032);
#3577=AXIS2_PLACEMENT_3D('',#5117,#4033,#4034);
#3578=AXIS2_PLACEMENT_3D('',#5118,#4035,#4036);
#3579=AXIS2_PLACEMENT_3D('',#5119,#4037,#4038);
#3580=AXIS2_PLACEMENT_3D('',#5121,#4040,#4041);
#3581=AXIS2_PLACEMENT_3D('',#5122,#4042,#4043);
#3582=AXIS2_PLACEMENT_3D('',#5143,#4045,#4046);
#3583=AXIS2_PLACEMENT_3D('',#5145,#4047,#4048);
#3584=AXIS2_PLACEMENT_3D('',#5147,#4049,#4050);
#3585=AXIS2_PLACEMENT_3D('',#5149,#4052,#4053);
#3586=AXIS2_PLACEMENT_3D('',#5151,#4054,#4055);
#3587=AXIS2_PLACEMENT_3D('',#5153,#4057,#4058);
#3588=AXIS2_PLACEMENT_3D('',#5155,#4059,#4060);
#3589=AXIS2_PLACEMENT_3D('',#5159,#4062,#4063);
#3590=AXIS2_PLACEMENT_3D('',#5161,#4065,#4066);
#3591=AXIS2_PLACEMENT_3D('',#5163,#4067,#4068);
#3592=AXIS2_PLACEMENT_3D('',#5165,#4070,#4071);
#3593=AXIS2_PLACEMENT_3D('',#5183,#4072,#4073);
#3594=AXIS2_PLACEMENT_3D('',#5185,#4074,#4075);
#3595=AXIS2_PLACEMENT_3D('',#5187,#4077,#4078);
#3596=AXIS2_PLACEMENT_3D('',#5189,#4079,#4080);
#3597=AXIS2_PLACEMENT_3D('',#5191,#4082,#4083);
#3598=AXIS2_PLACEMENT_3D('',#5193,#4084,#4085);
#3599=AXIS2_PLACEMENT_3D('',#5197,#4087,#4088);
#3600=AXIS2_PLACEMENT_3D('',#5199,#4090,#4091);
#3601=AXIS2_PLACEMENT_3D('',#5201,#4092,#4093);
#3602=AXIS2_PLACEMENT_3D('',#5203,#4095,#4096);
#3603=AXIS2_PLACEMENT_3D('',#5224,#4098,#4099);
#3604=AXIS2_PLACEMENT_3D('',#5226,#4100,#4101);
#3605=AXIS2_PLACEMENT_3D('',#5228,#4102,#4103);
#3606=AXIS2_PLACEMENT_3D('',#5230,#4105,#4106);
#3607=AXIS2_PLACEMENT_3D('',#5232,#4107,#4108);
#3608=AXIS2_PLACEMENT_3D('',#5234,#4110,#4111);
#3609=AXIS2_PLACEMENT_3D('',#5252,#4112,#4113);
#3610=AXIS2_PLACEMENT_3D('',#5254,#4114,#4115);
#3611=AXIS2_PLACEMENT_3D('',#5256,#4117,#4118);
#3612=AXIS2_PLACEMENT_3D('',#5258,#4119,#4120);
#3613=AXIS2_PLACEMENT_3D('',#5260,#4122,#4123);
#3614=AXIS2_PLACEMENT_3D('',#5262,#4124,#4125);
#3615=AXIS2_PLACEMENT_3D('',#5264,#4127,#4128);
#3616=AXIS2_PLACEMENT_3D('',#5266,#4129,#4130);
#3617=AXIS2_PLACEMENT_3D('',#5268,#4132,#4133);
#3618=AXIS2_PLACEMENT_3D('',#5269,#4134,#4135);
#3619=AXIS2_PLACEMENT_3D('',#5271,#4136,#4137);
#3620=AXIS2_PLACEMENT_3D('',#5273,#4139,#4140);
#3621=AXIS2_PLACEMENT_3D('',#5274,#4141,#4142);
#3622=AXIS2_PLACEMENT_3D('',#5276,#4144,#4145);
#3623=AXIS2_PLACEMENT_3D('',#5277,#4146,#4147);
#3624=AXIS2_PLACEMENT_3D('',#5279,#4148,#4149);
#3625=AXIS2_PLACEMENT_3D('',#5281,#4150,#4151);
#3626=AXIS2_PLACEMENT_3D('',#5282,#4152,#4153);
#3627=AXIS2_PLACEMENT_3D('',#5283,#4154,#4155);
#3628=AXIS2_PLACEMENT_3D('',#5285,#4156,#4157);
#3629=AXIS2_PLACEMENT_3D('',#5286,#4158,#4159);
#3630=AXIS2_PLACEMENT_3D('',#5288,#4160,#4161);
#3631=AXIS2_PLACEMENT_3D('',#5290,#4163,#4164);
#3632=AXIS2_PLACEMENT_3D('',#5292,#4165,#4166);
#3633=AXIS2_PLACEMENT_3D('',#5294,#4168,#4169);
#3634=AXIS2_PLACEMENT_3D('',#5296,#4170,#4171);
#3635=AXIS2_PLACEMENT_3D('',#5298,#4173,#4174);
#3636=AXIS2_PLACEMENT_3D('',#5299,#4175,#4176);
#3637=AXIS2_PLACEMENT_3D('',#5301,#4177,#4178);
#3638=AXIS2_PLACEMENT_3D('',#5303,#4179,#4180);
#3639=AXIS2_PLACEMENT_3D('',#5304,#4181,#4182);
#3640=AXIS2_PLACEMENT_3D('',#5305,#4183,#4184);
#3641=AXIS2_PLACEMENT_3D('',#5307,#4186,#4187);
#3642=AXIS2_PLACEMENT_3D('',#5308,#4188,#4189);
#3643=AXIS2_PLACEMENT_3D('',#5329,#4191,#4192);
#3644=AXIS2_PLACEMENT_3D('',#5331,#4193,#4194);
#3645=AXIS2_PLACEMENT_3D('',#5333,#4195,#4196);
#3646=AXIS2_PLACEMENT_3D('',#5335,#4198,#4199);
#3647=AXIS2_PLACEMENT_3D('',#5337,#4200,#4201);
#3648=AXIS2_PLACEMENT_3D('',#5339,#4203,#4204);
#3649=AXIS2_PLACEMENT_3D('',#5341,#4205,#4206);
#3650=AXIS2_PLACEMENT_3D('',#5345,#4208,#4209);
#3651=AXIS2_PLACEMENT_3D('',#5347,#4211,#4212);
#3652=AXIS2_PLACEMENT_3D('',#5349,#4213,#4214);
#3653=AXIS2_PLACEMENT_3D('',#5351,#4216,#4217);
#3654=AXIS2_PLACEMENT_3D('',#5369,#4218,#4219);
#3655=AXIS2_PLACEMENT_3D('',#5371,#4220,#4221);
#3656=AXIS2_PLACEMENT_3D('',#5373,#4223,#4224);
#3657=AXIS2_PLACEMENT_3D('',#5375,#4225,#4226);
#3658=AXIS2_PLACEMENT_3D('',#5377,#4228,#4229);
#3659=AXIS2_PLACEMENT_3D('',#5379,#4230,#4231);
#3660=AXIS2_PLACEMENT_3D('',#5383,#4233,#4234);
#3661=AXIS2_PLACEMENT_3D('',#5385,#4236,#4237);
#3662=AXIS2_PLACEMENT_3D('',#5387,#4238,#4239);
#3663=AXIS2_PLACEMENT_3D('',#5389,#4241,#4242);
#3664=AXIS2_PLACEMENT_3D('',#5410,#4244,#4245);
#3665=AXIS2_PLACEMENT_3D('',#5412,#4246,#4247);
#3666=AXIS2_PLACEMENT_3D('',#5414,#4248,#4249);
#3667=AXIS2_PLACEMENT_3D('',#5416,#4251,#4252);
#3668=AXIS2_PLACEMENT_3D('',#5418,#4253,#4254);
#3669=AXIS2_PLACEMENT_3D('',#5420,#4256,#4257);
#3670=AXIS2_PLACEMENT_3D('',#5438,#4258,#4259);
#3671=AXIS2_PLACEMENT_3D('',#5440,#4260,#4261);
#3672=AXIS2_PLACEMENT_3D('',#5442,#4263,#4264);
#3673=AXIS2_PLACEMENT_3D('',#5444,#4265,#4266);
#3674=AXIS2_PLACEMENT_3D('',#5446,#4268,#4269);
#3675=AXIS2_PLACEMENT_3D('',#5448,#4270,#4271);
#3676=AXIS2_PLACEMENT_3D('',#5450,#4273,#4274);
#3677=AXIS2_PLACEMENT_3D('',#5452,#4275,#4276);
#3678=AXIS2_PLACEMENT_3D('',#5454,#4278,#4279);
#3679=AXIS2_PLACEMENT_3D('',#5455,#4280,#4281);
#3680=AXIS2_PLACEMENT_3D('',#5457,#4282,#4283);
#3681=AXIS2_PLACEMENT_3D('',#5459,#4285,#4286);
#3682=AXIS2_PLACEMENT_3D('',#5460,#4287,#4288);
#3683=AXIS2_PLACEMENT_3D('',#5462,#4290,#4291);
#3684=AXIS2_PLACEMENT_3D('',#5463,#4292,#4293);
#3685=AXIS2_PLACEMENT_3D('',#5465,#4294,#4295);
#3686=AXIS2_PLACEMENT_3D('',#5467,#4296,#4297);
#3687=AXIS2_PLACEMENT_3D('',#5468,#4298,#4299);
#3688=AXIS2_PLACEMENT_3D('',#5469,#4300,#4301);
#3689=AXIS2_PLACEMENT_3D('',#5471,#4302,#4303);
#3690=AXIS2_PLACEMENT_3D('',#5472,#4304,#4305);
#3691=AXIS2_PLACEMENT_3D('',#5474,#4306,#4307);
#3692=AXIS2_PLACEMENT_3D('',#5476,#4309,#4310);
#3693=AXIS2_PLACEMENT_3D('',#5478,#4311,#4312);
#3694=AXIS2_PLACEMENT_3D('',#5480,#4314,#4315);
#3695=AXIS2_PLACEMENT_3D('',#5482,#4316,#4317);
#3696=AXIS2_PLACEMENT_3D('',#5484,#4319,#4320);
#3697=AXIS2_PLACEMENT_3D('',#5485,#4321,#4322);
#3698=AXIS2_PLACEMENT_3D('',#5487,#4323,#4324);
#3699=AXIS2_PLACEMENT_3D('',#5489,#4325,#4326);
#3700=AXIS2_PLACEMENT_3D('',#5490,#4327,#4328);
#3701=AXIS2_PLACEMENT_3D('',#5491,#4329,#4330);
#3702=AXIS2_PLACEMENT_3D('',#5493,#4332,#4333);
#3703=AXIS2_PLACEMENT_3D('',#5494,#4334,#4335);
#3704=AXIS2_PLACEMENT_3D('',#5515,#4337,#4338);
#3705=AXIS2_PLACEMENT_3D('',#5517,#4339,#4340);
#3706=AXIS2_PLACEMENT_3D('',#5519,#4341,#4342);
#3707=AXIS2_PLACEMENT_3D('',#5521,#4344,#4345);
#3708=AXIS2_PLACEMENT_3D('',#5523,#4346,#4347);
#3709=AXIS2_PLACEMENT_3D('',#5525,#4349,#4350);
#3710=AXIS2_PLACEMENT_3D('',#5527,#4351,#4352);
#3711=AXIS2_PLACEMENT_3D('',#5531,#4354,#4355);
#3712=AXIS2_PLACEMENT_3D('',#5533,#4357,#4358);
#3713=AXIS2_PLACEMENT_3D('',#5535,#4359,#4360);
#3714=AXIS2_PLACEMENT_3D('',#5537,#4362,#4363);
#3715=AXIS2_PLACEMENT_3D('',#5555,#4364,#4365);
#3716=AXIS2_PLACEMENT_3D('',#5557,#4366,#4367);
#3717=AXIS2_PLACEMENT_3D('',#5559,#4369,#4370);
#3718=AXIS2_PLACEMENT_3D('',#5561,#4371,#4372);
#3719=AXIS2_PLACEMENT_3D('',#5563,#4374,#4375);
#3720=AXIS2_PLACEMENT_3D('',#5565,#4376,#4377);
#3721=AXIS2_PLACEMENT_3D('',#5569,#4379,#4380);
#3722=AXIS2_PLACEMENT_3D('',#5571,#4382,#4383);
#3723=AXIS2_PLACEMENT_3D('',#5573,#4384,#4385);
#3724=AXIS2_PLACEMENT_3D('',#5575,#4387,#4388);
#3725=AXIS2_PLACEMENT_3D('',#5596,#4390,#4391);
#3726=AXIS2_PLACEMENT_3D('',#5598,#4392,#4393);
#3727=AXIS2_PLACEMENT_3D('',#5600,#4394,#4395);
#3728=AXIS2_PLACEMENT_3D('',#5602,#4397,#4398);
#3729=AXIS2_PLACEMENT_3D('',#5604,#4399,#4400);
#3730=AXIS2_PLACEMENT_3D('',#5606,#4402,#4403);
#3731=AXIS2_PLACEMENT_3D('',#5624,#4404,#4405);
#3732=AXIS2_PLACEMENT_3D('',#5626,#4406,#4407);
#3733=AXIS2_PLACEMENT_3D('',#5628,#4409,#4410);
#3734=AXIS2_PLACEMENT_3D('',#5630,#4411,#4412);
#3735=AXIS2_PLACEMENT_3D('',#5632,#4414,#4415);
#3736=AXIS2_PLACEMENT_3D('',#5634,#4416,#4417);
#3737=AXIS2_PLACEMENT_3D('',#5636,#4419,#4420);
#3738=AXIS2_PLACEMENT_3D('',#5638,#4421,#4422);
#3739=AXIS2_PLACEMENT_3D('',#5640,#4424,#4425);
#3740=AXIS2_PLACEMENT_3D('',#5641,#4426,#4427);
#3741=AXIS2_PLACEMENT_3D('',#5643,#4428,#4429);
#3742=AXIS2_PLACEMENT_3D('',#5645,#4431,#4432);
#3743=AXIS2_PLACEMENT_3D('',#5646,#4433,#4434);
#3744=AXIS2_PLACEMENT_3D('',#5648,#4436,#4437);
#3745=AXIS2_PLACEMENT_3D('',#5649,#4438,#4439);
#3746=AXIS2_PLACEMENT_3D('',#5651,#4440,#4441);
#3747=AXIS2_PLACEMENT_3D('',#5653,#4442,#4443);
#3748=AXIS2_PLACEMENT_3D('',#5654,#4444,#4445);
#3749=AXIS2_PLACEMENT_3D('',#5655,#4446,#4447);
#3750=AXIS2_PLACEMENT_3D('',#5657,#4448,#4449);
#3751=AXIS2_PLACEMENT_3D('',#5658,#4450,#4451);
#3752=AXIS2_PLACEMENT_3D('',#5660,#4452,#4453);
#3753=AXIS2_PLACEMENT_3D('',#5662,#4455,#4456);
#3754=AXIS2_PLACEMENT_3D('',#5664,#4457,#4458);
#3755=AXIS2_PLACEMENT_3D('',#5666,#4460,#4461);
#3756=AXIS2_PLACEMENT_3D('',#5668,#4462,#4463);
#3757=AXIS2_PLACEMENT_3D('',#5670,#4465,#4466);
#3758=AXIS2_PLACEMENT_3D('',#5671,#4467,#4468);
#3759=AXIS2_PLACEMENT_3D('',#5673,#4469,#4470);
#3760=AXIS2_PLACEMENT_3D('',#5675,#4471,#4472);
#3761=AXIS2_PLACEMENT_3D('',#5676,#4473,#4474);
#3762=AXIS2_PLACEMENT_3D('',#5677,#4475,#4476);
#3763=AXIS2_PLACEMENT_3D('',#5679,#4478,#4479);
#3764=AXIS2_PLACEMENT_3D('',#5680,#4480,#4481);
#3765=AXIS2_PLACEMENT_3D('',#5689,#4486,#4487);
#3766=AXIS2_PLACEMENT_3D('',#5695,#4491,#4492);
#3767=AXIS2_PLACEMENT_3D('',#5701,#4496,#4497);
#3768=AXIS2_PLACEMENT_3D('',#5703,#4499,#4500);
#3769=AXIS2_PLACEMENT_3D('',#5714,#4506,#4507);
#3770=AXIS2_PLACEMENT_3D('',#5716,#4508,#4509);
#3771=AXIS2_PLACEMENT_3D('',#5717,#4510,#4511);
#3772=AXIS2_PLACEMENT_3D('',#5723,#4515,#4516);
#3773=AXIS2_PLACEMENT_3D('',#5730,#4520,#4521);
#3774=AXIS2_PLACEMENT_3D('',#5732,#4522,#4523);
#3775=AXIS2_PLACEMENT_3D('',#5733,#4524,#4525);
#3776=AXIS2_PLACEMENT_3D('',#5735,#4527,#4528);
#3777=AXIS2_PLACEMENT_3D('',#5737,#4530,#4531);
#3778=AXIS2_PLACEMENT_3D('',#5739,#4533,#4534);
#3779=AXIS2_PLACEMENT_3D('',#5741,#4536,#4537);
#3780=AXIS2_PLACEMENT_3D('',#5742,#4538,#4539);
#3781=AXIS2_PLACEMENT_3D('',#5743,#4540,#4541);
#3782=AXIS2_PLACEMENT_3D('',#5752,#4546,#4547);
#3783=AXIS2_PLACEMENT_3D('',#5758,#4551,#4552);
#3784=AXIS2_PLACEMENT_3D('',#5764,#4556,#4557);
#3785=AXIS2_PLACEMENT_3D('',#5766,#4559,#4560);
#3786=AXIS2_PLACEMENT_3D('',#5776,#4566,#4567);
#3787=AXIS2_PLACEMENT_3D('',#5778,#4568,#4569);
#3788=AXIS2_PLACEMENT_3D('',#5781,#4571,#4572);
#3789=AXIS2_PLACEMENT_3D('',#5782,#4573,#4574);
#3790=AXIS2_PLACEMENT_3D('',#5791,#4579,#4580);
#3791=AXIS2_PLACEMENT_3D('',#5800,#4585,#4586);
#3792=AXIS2_PLACEMENT_3D('',#5803,#4589,#4590);
#3793=AXIS2_PLACEMENT_3D('',#5813,#4596,#4597);
#3794=AXIS2_PLACEMENT_3D('',#5822,#4602,#4603);
#3795=AXIS2_PLACEMENT_3D('',#5828,#4607,#4608);
#3796=AXIS2_PLACEMENT_3D('',#5831,#4611,#4612);
#3797=AXIS2_PLACEMENT_3D('',#5832,#4613,#4614);
#3798=AXIS2_PLACEMENT_3D('',#5833,#4615,#4616);
#3799=AXIS2_PLACEMENT_3D('',#5842,#4621,#4622);
#3800=AXIS2_PLACEMENT_3D('',#5843,#4623,#4624);
#3801=AXIS2_PLACEMENT_3D('',#5844,#4625,#4626);
#3802=AXIS2_PLACEMENT_3D('',#5845,#4627,#4628);
#3803=AXIS2_PLACEMENT_3D('',#5851,#4632,#4633);
#3804=AXIS2_PLACEMENT_3D('',#5857,#4637,#4638);
#3805=AXIS2_PLACEMENT_3D('',#5858,#4639,#4640);
#3806=AXIS2_PLACEMENT_3D('',#5860,#4642,#4643);
#3807=AXIS2_PLACEMENT_3D('',#5864,#4646,#4647);
#3808=AXIS2_PLACEMENT_3D('',#5866,#4649,#4650);
#3809=AXIS2_PLACEMENT_3D('',#5868,#4652,#4653);
#3810=AXIS2_PLACEMENT_3D('',#5869,#4654,#4655);
#3811=AXIS2_PLACEMENT_3D('',#5870,#4656,#4657);
#3812=AXIS2_PLACEMENT_3D('',#5879,#4662,#4663);
#3813=AXIS2_PLACEMENT_3D('',#5885,#4667,#4668);
#3814=AXIS2_PLACEMENT_3D('',#5891,#4672,#4673);
#3815=AXIS2_PLACEMENT_3D('',#5893,#4675,#4676);
#3816=AXIS2_PLACEMENT_3D('',#5903,#4682,#4683);
#3817=AXIS2_PLACEMENT_3D('',#5910,#4687,#4688);
#3818=AXIS2_PLACEMENT_3D('',#5912,#4689,#4690);
#3819=AXIS2_PLACEMENT_3D('',#5913,#4691,#4692);
#3820=AXIS2_PLACEMENT_3D('',#5917,#4695,#4696);
#3821=AXIS2_PLACEMENT_3D('',#5922,#4699,#4700);
#3822=AXIS2_PLACEMENT_3D('',#5924,#4701,#4702);
#3823=AXIS2_PLACEMENT_3D('',#5925,#4703,#4704);
#3824=AXIS2_PLACEMENT_3D('',#5927,#4706,#4707);
#3825=AXIS2_PLACEMENT_3D('',#5929,#4709,#4710);
#3826=AXIS2_PLACEMENT_3D('',#5931,#4712,#4713);
#3827=AXIS2_PLACEMENT_3D('',#5932,#4714,#4715);
#3828=AXIS2_PLACEMENT_3D('',#5933,#4716,#4717);
#3829=AXIS2_PLACEMENT_3D('',#5942,#4722,#4723);
#3830=AXIS2_PLACEMENT_3D('',#5948,#4727,#4728);
#3831=AXIS2_PLACEMENT_3D('',#5954,#4732,#4733);
#3832=AXIS2_PLACEMENT_3D('',#5956,#4735,#4736);
#3833=AXIS2_PLACEMENT_3D('',#5966,#4742,#4743);
#3834=AXIS2_PLACEMENT_3D('',#5975,#4748,#4749);
#3835=AXIS2_PLACEMENT_3D('',#5981,#4753,#4754);
#3836=AXIS2_PLACEMENT_3D('',#5983,#4755,#4756);
#3837=AXIS2_PLACEMENT_3D('',#5986,#4758,#4759);
#3838=AXIS2_PLACEMENT_3D('',#5987,#4760,#4761);
#3839=AXIS2_PLACEMENT_3D('',#5991,#4763,#4764);
#3840=AXIS2_PLACEMENT_3D('',#6000,#4769,#4770);
#3841=AXIS2_PLACEMENT_3D('',#6002,#4772,#4773);
#3842=AXIS2_PLACEMENT_3D('',#6007,#4776,#4777);
#3843=AXIS2_PLACEMENT_3D('',#6008,#4778,#4779);
#3844=AXIS2_PLACEMENT_3D('',#6018,#4785,#4786);
#3845=AXIS2_PLACEMENT_3D('',#6022,#4788,#4789);
#3846=AXIS2_PLACEMENT_3D('',#6023,#4790,#4791);
#3847=AXIS2_PLACEMENT_3D('',#6024,#4792,#4793);
#3848=AXIS2_PLACEMENT_3D('',#6033,#4798,#4799);
#3849=AXIS2_PLACEMENT_3D('',#6036,#4802,#4803);
#3850=AXIS2_PLACEMENT_3D('',#6038,#4805,#4806);
#3851=AXIS2_PLACEMENT_3D('',#6040,#4808,#4809);
#3852=AXIS2_PLACEMENT_3D('',#6043,#4811,#4812);
#3853=AXIS2_PLACEMENT_3D('',#6044,#4813,#4814);
#3854=AXIS2_PLACEMENT_3D('',#6050,#4818,#4819);
#3855=AXIS2_PLACEMENT_3D('',#6052,#4821,#4822);
#3856=AXIS2_PLACEMENT_3D('',#6054,#4824,#4825);
#3857=AXIS2_PLACEMENT_3D('',#6056,#4826,#4827);
#3858=AXIS2_PLACEMENT_3D('',#6058,#4829,#4830);
#3859=AXIS2_PLACEMENT_3D('',#6060,#4832,#4833);
#3860=AXIS2_PLACEMENT_3D('',#6061,#4834,#4835);
#3861=AXIS2_PLACEMENT_3D('',#6853,#4836,#4837);
#3862=AXIS2_PLACEMENT_3D('',#6934,#4838,#4839);
#3863=AXIS2_PLACEMENT_3D('',#6935,#4840,#4841);
#3864=AXIS2_PLACEMENT_3D('',#6936,#4842,#4843);
#3865=AXIS2_PLACEMENT_3D('',#6937,#4844,#4845);
#3866=AXIS2_PLACEMENT_3D('',#6938,#4846,#4847);
#3867=AXIS2_PLACEMENT_3D('',#6947,#4852,#4853);
#3868=AXIS2_PLACEMENT_3D('',#6953,#4857,#4858);
#3869=AXIS2_PLACEMENT_3D('',#6959,#4862,#4863);
#3870=AXIS2_PLACEMENT_3D('',#6962,#4866,#4867);
#3871=AXIS2_PLACEMENT_3D('',#6971,#4872,#4873);
#3872=AXIS2_PLACEMENT_3D('',#6977,#4877,#4878);
#3873=AXIS2_PLACEMENT_3D('',#6981,#4881,#4882);
#3874=AXIS2_PLACEMENT_3D('',#6990,#4887,#4888);
#3875=AXIS2_PLACEMENT_3D('',#6996,#4892,#4893);
#3876=AXIS2_PLACEMENT_3D('',#7002,#4897,#4898);
#3877=AXIS2_PLACEMENT_3D('',#7005,#4901,#4902);
#3878=AXIS2_PLACEMENT_3D('',#7006,#4903,#4904);
#3879=AXIS2_PLACEMENT_3D('',#7010,#4907,#4908);
#3880=AXIS2_PLACEMENT_3D('',#7012,#4910,#4911);
#3881=AXIS2_PLACEMENT_3D('',#7013,#4912,#4913);
#3882=AXIS2_PLACEMENT_3D('',#7014,#4914,#4915);
#3883=AXIS2_PLACEMENT_3D('',#7015,#4916,#4917);
#3884=AXIS2_PLACEMENT_3D('',#7016,#4918,#4919);
#3885=AXIS2_PLACEMENT_3D('',#7017,#4920,#4921);
#3886=AXIS2_PLACEMENT_3D('',#7018,#4922,#4923);
#3887=AXIS2_PLACEMENT_3D('',#7019,#4924,#4925);
#3888=AXIS2_PLACEMENT_3D('',#7020,#4926,#4927);
#3889=AXIS2_PLACEMENT_3D('',#7021,#4928,#4929);
#3890=AXIS2_PLACEMENT_3D('',#7022,#4930,#4931);
#3891=AXIS2_PLACEMENT_3D('',#7023,#4932,#4933);
#3892=DIRECTION('axis',(0.,0.,1.));
#3893=DIRECTION('refdir',(1.,0.,0.));
#3894=DIRECTION('axis',(0.,0.,1.));
#3895=DIRECTION('refdir',(1.,0.,0.));
#3896=DIRECTION('center_axis',(0.,0.,-1.));
#3897=DIRECTION('ref_axis',(0.707106781186563,-0.707106781186532,0.));
#3898=DIRECTION('',(0.,0.,1.));
#3899=DIRECTION('center_axis',(-0.866025403784439,0.,-0.5));
#3900=DIRECTION('ref_axis',(0.5,0.,-0.866025403784439));
#3901=DIRECTION('center_axis',(0.,0.,-1.));
#3902=DIRECTION('ref_axis',(0.707106781186563,-0.707106781186532,0.));
#3903=DIRECTION('center_axis',(-2.54091264057109E-15,0.866025403784439,
-0.5));
#3904=DIRECTION('ref_axis',(1.43032168209504E-15,-0.5,-0.866025403784439));
#3905=DIRECTION('',(0.,0.,-1.));
#3906=DIRECTION('center_axis',(-1.,-4.30300426108057E-14,0.));
#3907=DIRECTION('ref_axis',(-4.30300426108057E-14,1.,0.));
#3908=DIRECTION('center_axis',(-1.,-4.30300426108057E-14,0.));
#3909=DIRECTION('ref_axis',(0.,0.,-1.));
#3910=DIRECTION('',(-2.15150213054029E-14,0.5,0.866025403784439));
#3911=DIRECTION('center_axis',(-2.54091264057109E-15,0.866025403784439,
-0.5));
#3912=DIRECTION('ref_axis',(1.,2.93399319404209E-15,0.));
#3913=DIRECTION('center_axis',(-2.54091264057109E-15,0.866025403784439,
-0.5));
#3914=DIRECTION('ref_axis',(0.,-0.5,-0.866025403784439));
#3915=DIRECTION('',(-1.,-2.93399319404209E-15,0.));
#3916=DIRECTION('center_axis',(-2.54091264057109E-15,0.866025403784439,
-0.5));
#3917=DIRECTION('ref_axis',(1.46699659702056E-15,-0.5,-0.866025403784439));
#3918=DIRECTION('',(-1.73044443434865E-14,-0.5,-0.866025403784439));
#3919=DIRECTION('center_axis',(1.,-3.4608888686973E-14,0.));
#3920=DIRECTION('ref_axis',(-3.4608888686973E-14,-1.,0.));
#3921=DIRECTION('center_axis',(1.,-3.4608888686973E-14,0.));
#3922=DIRECTION('ref_axis',(0.,0.,1.));
#3923=DIRECTION('',(0.,0.,1.));
#3924=DIRECTION('center_axis',(0.,0.,-1.));
#3925=DIRECTION('ref_axis',(-0.707106781186546,-0.707106781186549,0.));
#3926=DIRECTION('center_axis',(0.,0.,-1.));
#3927=DIRECTION('ref_axis',(-0.707106781186546,-0.707106781186549,0.));
#3928=DIRECTION('center_axis',(0.866025403784439,0.,-0.5));
#3929=DIRECTION('ref_axis',(-0.5,-3.66749149255139E-17,-0.866025403784439));
#3930=DIRECTION('',(0.,0.,-1.));
#3931=DIRECTION('center_axis',(-4.04626176340286E-14,1.,0.));
#3932=DIRECTION('ref_axis',(1.,4.04626176340286E-14,0.));
#3933=DIRECTION('center_axis',(-4.04626176340286E-14,1.,0.));
#3934=DIRECTION('ref_axis',(0.,0.,-1.));
#3935=DIRECTION('',(0.5,2.02313088170143E-14,0.866025403784439));
#3936=DIRECTION('center_axis',(0.866025403784439,0.,-0.5));
#3937=DIRECTION('ref_axis',(0.,-1.,0.));
#3938=DIRECTION('center_axis',(0.866025403784439,0.,-0.5));
#3939=DIRECTION('ref_axis',(0.5,0.,0.866025403784439));
#3940=DIRECTION('',(0.,1.,0.));
#3941=DIRECTION('center_axis',(0.866025403784439,0.,-0.5));
#3942=DIRECTION('ref_axis',(-0.5,3.66749149255139E-17,-0.866025403784439));
#3943=DIRECTION('',(-0.5,2.39626331165986E-16,-0.866025403784439));
#3944=DIRECTION('center_axis',(-4.79252662331972E-16,-1.,0.));
#3945=DIRECTION('ref_axis',(-1.,4.79252662331972E-16,0.));
#3946=DIRECTION('center_axis',(-4.79252662331972E-16,-1.,0.));
#3947=DIRECTION('ref_axis',(0.,0.,1.));
#3948=DIRECTION('',(0.,0.,1.));
#3949=DIRECTION('center_axis',(0.,0.,-1.));
#3950=DIRECTION('ref_axis',(0.70710678118653,0.707106781186565,0.));
#3951=DIRECTION('',(0.,0.,1.));
#3952=DIRECTION('center_axis',(-1.27045632028555E-15,-0.866025403784439,
-0.5));
#3953=DIRECTION('ref_axis',(6.96823383584764E-16,0.5,-0.866025403784439));
#3954=DIRECTION('center_axis',(0.,0.,-1.));
#3955=DIRECTION('ref_axis',(0.70710678118653,0.707106781186565,0.));
#3956=DIRECTION('center_axis',(-0.866025403784439,0.,-0.5));
#3957=DIRECTION('ref_axis',(0.5,3.66749149255139E-17,-0.866025403784439));
#3958=DIRECTION('',(0.,0.,-1.));
#3959=DIRECTION('center_axis',(5.35736011821097E-14,-1.,0.));
#3960=DIRECTION('ref_axis',(-1.,-5.35736011821097E-14,0.));
#3961=DIRECTION('center_axis',(5.35736011821097E-14,-1.,0.));
#3962=DIRECTION('ref_axis',(0.,0.,1.));
#3963=DIRECTION('',(-0.5,-2.67868005910549E-14,0.866025403784439));
#3964=DIRECTION('center_axis',(0.,0.,-1.));
#3965=DIRECTION('ref_axis',(-0.707106781186557,0.707106781186538,0.));
#3966=DIRECTION('center_axis',(0.,0.,-1.));
#3967=DIRECTION('ref_axis',(-0.707106781186557,0.707106781186538,0.));
#3968=DIRECTION('center_axis',(-1.27045632028555E-15,-0.866025403784439,
-0.5));
#3969=DIRECTION('ref_axis',(7.33498298510278E-16,0.5,-0.866025403784439));
#3970=DIRECTION('',(0.,0.,-1.));
#3971=DIRECTION('center_axis',(1.,2.81047454124667E-14,0.));
#3972=DIRECTION('ref_axis',(2.81047454124667E-14,-1.,0.));
#3973=DIRECTION('center_axis',(1.,2.81047454124667E-14,0.));
#3974=DIRECTION('ref_axis',(0.,0.,1.));
#3975=DIRECTION('',(1.40523727062334E-14,-0.5,0.866025403784439));
#3976=DIRECTION('center_axis',(0.,1.,0.));
#3977=DIRECTION('ref_axis',(1.,0.,0.));
#3978=DIRECTION('center_axis',(0.,1.,0.));
#3979=DIRECTION('ref_axis',(0.,0.,-1.));
#3980=DIRECTION('',(0.5,0.,-0.866025403784439));
#3981=DIRECTION('center_axis',(-0.866025403784439,0.,-0.5));
#3982=DIRECTION('ref_axis',(0.,1.,0.));
#3983=DIRECTION('center_axis',(-0.866025403784439,0.,-0.5));
#3984=DIRECTION('ref_axis',(0.5,0.,-0.866025403784439));
#3985=DIRECTION('',(0.,-1.,0.));
#3986=DIRECTION('center_axis',(-0.866025403784439,0.,-0.5));
#3987=DIRECTION('ref_axis',(0.5,0.,-0.866025403784439));
#3988=DIRECTION('center_axis',(-1.,3.8682536316795E-15,0.));
#3989=DIRECTION('ref_axis',(3.8682536316795E-15,1.,0.));
#3990=DIRECTION('center_axis',(-1.,3.8682536316795E-15,0.));
#3991=DIRECTION('ref_axis',(0.,0.,-1.));
#3992=DIRECTION('',(1.93412681583975E-15,0.5,-0.866025403784439));
#3993=DIRECTION('center_axis',(-1.27045632028555E-15,-0.866025403784439,
-0.5));
#3994=DIRECTION('ref_axis',(-1.,1.46699659702105E-15,0.));
#3995=DIRECTION('center_axis',(-1.27045632028555E-15,-0.866025403784439,
-0.5));
#3996=DIRECTION('ref_axis',(0.,-0.5,0.866025403784439));
#3997=DIRECTION('',(1.,-1.46699659702105E-15,0.));
#3998=DIRECTION('center_axis',(0.,0.,-1.));
#3999=DIRECTION('ref_axis',(-1.,0.,0.));
#4000=DIRECTION('center_axis',(0.,0.,-1.));
#4001=DIRECTION('ref_axis',(-1.,0.,0.));
#4002=DIRECTION('center_axis',(0.,0.,-1.));
#4003=DIRECTION('ref_axis',(1.,0.,0.));
#4004=DIRECTION('center_axis',(-1.22464679914735E-16,-1.,0.));
#4005=DIRECTION('ref_axis',(1.,-1.22464679914735E-16,0.));
#4006=DIRECTION('center_axis',(0.,0.,1.));
#4007=DIRECTION('ref_axis',(1.,0.,0.));
#4008=DIRECTION('center_axis',(0.,0.,-1.));
#4009=DIRECTION('ref_axis',(-1.,0.,0.));
#4010=DIRECTION('center_axis',(0.,0.,-1.));
#4011=DIRECTION('ref_axis',(1.,0.,0.));
#4012=DIRECTION('center_axis',(0.,0.,-1.));
#4013=DIRECTION('ref_axis',(-1.,0.,0.));
#4014=DIRECTION('center_axis',(0.,0.,-1.));
#4015=DIRECTION('ref_axis',(1.,0.,0.));
#4016=DIRECTION('',(0.,0.,1.));
#4017=DIRECTION('center_axis',(0.,0.,-1.));
#4018=DIRECTION('ref_axis',(-1.,0.,0.));
#4019=DIRECTION('center_axis',(0.,0.,-1.));
#4020=DIRECTION('ref_axis',(-1.,0.,0.));
#4021=DIRECTION('',(-0.258819045102519,3.16961915143174E-17,0.965925826289069));
#4022=DIRECTION('center_axis',(0.,0.,-1.));
#4023=DIRECTION('ref_axis',(-1.,0.,0.));
#4024=DIRECTION('center_axis',(0.,0.,1.));
#4025=DIRECTION('ref_axis',(-1.,0.,0.));
#4026=DIRECTION('',(0.,0.,1.));
#4027=DIRECTION('center_axis',(0.,0.,-1.));
#4028=DIRECTION('ref_axis',(-1.,0.,0.));
#4029=DIRECTION('center_axis',(6.12323399573676E-17,0.,1.));
#4030=DIRECTION('ref_axis',(1.,0.,0.));
#4031=DIRECTION('center_axis',(1.22464679914735E-16,-1.,0.));
#4032=DIRECTION('ref_axis',(-1.,-1.22464679914735E-16,0.));
#4033=DIRECTION('center_axis',(0.,0.,-1.));
#4034=DIRECTION('ref_axis',(1.,0.,0.));
#4035=DIRECTION('center_axis',(0.,0.,-1.));
#4036=DIRECTION('ref_axis',(1.,0.,0.));
#4037=DIRECTION('center_axis',(0.,0.,-1.));
#4038=DIRECTION('ref_axis',(-1.,0.,0.));
#4039=DIRECTION('',(-0.0871557427578718,1.06735001395738E-17,0.996194698090852));
#4040=DIRECTION('axis',(0.,0.,1.));
#4041=DIRECTION('refdir',(1.,0.,0.));
#4042=DIRECTION('center_axis',(0.,0.,-1.));
#4043=DIRECTION('ref_axis',(0.707106781186563,-0.707106781186532,0.));
#4044=DIRECTION('',(0.,0.,1.));
#4045=DIRECTION('center_axis',(-0.866025403784439,0.,-0.5));
#4046=DIRECTION('ref_axis',(0.5,0.,-0.866025403784439));
#4047=DIRECTION('center_axis',(0.,0.,-1.));
#4048=DIRECTION('ref_axis',(0.707106781186563,-0.707106781186532,0.));
#4049=DIRECTION('center_axis',(-2.54091264057109E-15,0.866025403784439,
-0.5));
#4050=DIRECTION('ref_axis',(1.43032168209504E-15,-0.5,-0.866025403784439));
#4051=DIRECTION('',(0.,0.,-1.));
#4052=DIRECTION('center_axis',(-1.,-4.30300426108057E-14,0.));
#4053=DIRECTION('ref_axis',(-4.30300426108057E-14,1.,0.));
#4054=DIRECTION('center_axis',(-1.,-4.30300426108057E-14,0.));
#4055=DIRECTION('ref_axis',(0.,0.,-1.));
#4056=DIRECTION('',(-2.15150213054029E-14,0.5,0.866025403784439));
#4057=DIRECTION('center_axis',(-2.54091264057109E-15,0.866025403784439,
-0.5));
#4058=DIRECTION('ref_axis',(1.,2.93399319404209E-15,0.));
#4059=DIRECTION('center_axis',(-2.54091264057109E-15,0.866025403784439,
-0.5));
#4060=DIRECTION('ref_axis',(0.,-0.5,-0.866025403784439));
#4061=DIRECTION('',(-1.,-2.93399319404209E-15,0.));
#4062=DIRECTION('center_axis',(-2.54091264057109E-15,0.866025403784439,
-0.5));
#4063=DIRECTION('ref_axis',(1.46699659702056E-15,-0.5,-0.866025403784439));
#4064=DIRECTION('',(-1.73044443434865E-14,-0.5,-0.866025403784439));
#4065=DIRECTION('center_axis',(1.,-3.4608888686973E-14,0.));
#4066=DIRECTION('ref_axis',(-3.4608888686973E-14,-1.,0.));
#4067=DIRECTION('center_axis',(1.,-3.4608888686973E-14,0.));
#4068=DIRECTION('ref_axis',(0.,0.,1.));
#4069=DIRECTION('',(0.,0.,1.));
#4070=DIRECTION('center_axis',(0.,0.,-1.));
#4071=DIRECTION('ref_axis',(-0.707106781186546,-0.707106781186549,0.));
#4072=DIRECTION('center_axis',(0.,0.,-1.));
#4073=DIRECTION('ref_axis',(-0.707106781186546,-0.707106781186549,0.));
#4074=DIRECTION('center_axis',(0.866025403784439,0.,-0.5));
#4075=DIRECTION('ref_axis',(-0.5,-3.66749149255139E-17,-0.866025403784439));
#4076=DIRECTION('',(0.,0.,-1.));
#4077=DIRECTION('center_axis',(-4.04626176340286E-14,1.,0.));
#4078=DIRECTION('ref_axis',(1.,4.04626176340286E-14,0.));
#4079=DIRECTION('center_axis',(-4.04626176340286E-14,1.,0.));
#4080=DIRECTION('ref_axis',(0.,0.,-1.));
#4081=DIRECTION('',(0.5,2.02313088170143E-14,0.866025403784439));
#4082=DIRECTION('center_axis',(0.866025403784439,0.,-0.5));
#4083=DIRECTION('ref_axis',(0.,-1.,0.));
#4084=DIRECTION('center_axis',(0.866025403784439,0.,-0.5));
#4085=DIRECTION('ref_axis',(0.5,0.,0.866025403784439));
#4086=DIRECTION('',(0.,1.,0.));
#4087=DIRECTION('center_axis',(0.866025403784439,0.,-0.5));
#4088=DIRECTION('ref_axis',(-0.5,3.66749149255139E-17,-0.866025403784439));
#4089=DIRECTION('',(-0.5,2.39626331165986E-16,-0.866025403784439));
#4090=DIRECTION('center_axis',(-4.79252662331972E-16,-1.,0.));
#4091=DIRECTION('ref_axis',(-1.,4.79252662331972E-16,0.));
#4092=DIRECTION('center_axis',(-4.79252662331972E-16,-1.,0.));
#4093=DIRECTION('ref_axis',(0.,0.,1.));
#4094=DIRECTION('',(0.,0.,1.));
#4095=DIRECTION('center_axis',(0.,0.,-1.));
#4096=DIRECTION('ref_axis',(0.70710678118653,0.707106781186565,0.));
#4097=DIRECTION('',(0.,0.,1.));
#4098=DIRECTION('center_axis',(-1.27045632028555E-15,-0.866025403784439,
-0.5));
#4099=DIRECTION('ref_axis',(6.96823383584764E-16,0.5,-0.866025403784439));
#4100=DIRECTION('center_axis',(0.,0.,-1.));
#4101=DIRECTION('ref_axis',(0.70710678118653,0.707106781186565,0.));
#4102=DIRECTION('center_axis',(-0.866025403784439,0.,-0.5));
#4103=DIRECTION('ref_axis',(0.5,3.66749149255139E-17,-0.866025403784439));
#4104=DIRECTION('',(0.,0.,-1.));
#4105=DIRECTION('center_axis',(5.35736011821097E-14,-1.,0.));
#4106=DIRECTION('ref_axis',(-1.,-5.35736011821097E-14,0.));
#4107=DIRECTION('center_axis',(5.35736011821097E-14,-1.,0.));
#4108=DIRECTION('ref_axis',(0.,0.,1.));
#4109=DIRECTION('',(-0.5,-2.67868005910549E-14,0.866025403784439));
#4110=DIRECTION('center_axis',(0.,0.,-1.));
#4111=DIRECTION('ref_axis',(-0.707106781186557,0.707106781186538,0.));
#4112=DIRECTION('center_axis',(0.,0.,-1.));
#4113=DIRECTION('ref_axis',(-0.707106781186557,0.707106781186538,0.));
#4114=DIRECTION('center_axis',(-1.27045632028555E-15,-0.866025403784439,
-0.5));
#4115=DIRECTION('ref_axis',(7.33498298510278E-16,0.5,-0.866025403784439));
#4116=DIRECTION('',(0.,0.,-1.));
#4117=DIRECTION('center_axis',(1.,2.81047454124667E-14,0.));
#4118=DIRECTION('ref_axis',(2.81047454124667E-14,-1.,0.));
#4119=DIRECTION('center_axis',(1.,2.81047454124667E-14,0.));
#4120=DIRECTION('ref_axis',(0.,0.,1.));
#4121=DIRECTION('',(1.40523727062334E-14,-0.5,0.866025403784439));
#4122=DIRECTION('center_axis',(0.,1.,0.));
#4123=DIRECTION('ref_axis',(1.,0.,0.));
#4124=DIRECTION('center_axis',(0.,1.,0.));
#4125=DIRECTION('ref_axis',(0.,0.,-1.));
#4126=DIRECTION('',(0.5,0.,-0.866025403784439));
#4127=DIRECTION('center_axis',(-0.866025403784439,0.,-0.5));
#4128=DIRECTION('ref_axis',(0.,1.,0.));
#4129=DIRECTION('center_axis',(-0.866025403784439,0.,-0.5));
#4130=DIRECTION('ref_axis',(0.5,0.,-0.866025403784439));
#4131=DIRECTION('',(0.,-1.,0.));
#4132=DIRECTION('center_axis',(-0.866025403784439,0.,-0.5));
#4133=DIRECTION('ref_axis',(0.5,0.,-0.866025403784439));
#4134=DIRECTION('center_axis',(-1.,3.8682536316795E-15,0.));
#4135=DIRECTION('ref_axis',(3.8682536316795E-15,1.,0.));
#4136=DIRECTION('center_axis',(-1.,3.8682536316795E-15,0.));
#4137=DIRECTION('ref_axis',(0.,0.,-1.));
#4138=DIRECTION('',(1.93412681583975E-15,0.5,-0.866025403784439));
#4139=DIRECTION('center_axis',(-1.27045632028555E-15,-0.866025403784439,
-0.5));
#4140=DIRECTION('ref_axis',(-1.,1.46699659702105E-15,0.));
#4141=DIRECTION('center_axis',(-1.27045632028555E-15,-0.866025403784439,
-0.5));
#4142=DIRECTION('ref_axis',(0.,-0.5,0.866025403784439));
#4143=DIRECTION('',(1.,-1.46699659702105E-15,0.));
#4144=DIRECTION('center_axis',(0.,0.,-1.));
#4145=DIRECTION('ref_axis',(-1.,0.,0.));
#4146=DIRECTION('center_axis',(0.,0.,-1.));
#4147=DIRECTION('ref_axis',(-1.,0.,0.));
#4148=DIRECTION('center_axis',(0.,0.,-1.));
#4149=DIRECTION('ref_axis',(1.,0.,0.));
#4150=DIRECTION('center_axis',(-1.22464679914735E-16,-1.,0.));
#4151=DIRECTION('ref_axis',(1.,-1.22464679914735E-16,0.));
#4152=DIRECTION('center_axis',(0.,0.,1.));
#4153=DIRECTION('ref_axis',(1.,0.,0.));
#4154=DIRECTION('center_axis',(0.,0.,-1.));
#4155=DIRECTION('ref_axis',(-1.,0.,0.));
#4156=DIRECTION('center_axis',(0.,0.,-1.));
#4157=DIRECTION('ref_axis',(1.,0.,0.));
#4158=DIRECTION('center_axis',(0.,0.,-1.));
#4159=DIRECTION('ref_axis',(-1.,0.,0.));
#4160=DIRECTION('center_axis',(0.,0.,-1.));
#4161=DIRECTION('ref_axis',(1.,0.,0.));
#4162=DIRECTION('',(0.,0.,1.));
#4163=DIRECTION('center_axis',(0.,0.,-1.));
#4164=DIRECTION('ref_axis',(-1.,0.,0.));
#4165=DIRECTION('center_axis',(0.,0.,-1.));
#4166=DIRECTION('ref_axis',(-1.,0.,0.));
#4167=DIRECTION('',(-0.258819045102519,3.16961915143174E-17,0.965925826289069));
#4168=DIRECTION('center_axis',(0.,0.,-1.));
#4169=DIRECTION('ref_axis',(-1.,0.,0.));
#4170=DIRECTION('center_axis',(0.,0.,1.));
#4171=DIRECTION('ref_axis',(-1.,0.,0.));
#4172=DIRECTION('',(0.,0.,1.));
#4173=DIRECTION('center_axis',(0.,0.,-1.));
#4174=DIRECTION('ref_axis',(-1.,0.,0.));
#4175=DIRECTION('center_axis',(6.12323399573676E-17,0.,1.));
#4176=DIRECTION('ref_axis',(1.,0.,0.));
#4177=DIRECTION('center_axis',(1.22464679914735E-16,-1.,0.));
#4178=DIRECTION('ref_axis',(-1.,-1.22464679914735E-16,0.));
#4179=DIRECTION('center_axis',(0.,0.,-1.));
#4180=DIRECTION('ref_axis',(1.,0.,0.));
#4181=DIRECTION('center_axis',(0.,0.,-1.));
#4182=DIRECTION('ref_axis',(1.,0.,0.));
#4183=DIRECTION('center_axis',(0.,0.,-1.));
#4184=DIRECTION('ref_axis',(-1.,0.,0.));
#4185=DIRECTION('',(-0.0871557427578718,1.06735001395738E-17,0.996194698090852));
#4186=DIRECTION('axis',(0.,0.,1.));
#4187=DIRECTION('refdir',(1.,0.,0.));
#4188=DIRECTION('center_axis',(0.,0.,-1.));
#4189=DIRECTION('ref_axis',(0.707106781186563,-0.707106781186532,0.));
#4190=DIRECTION('',(0.,0.,1.));
#4191=DIRECTION('center_axis',(-0.866025403784439,0.,-0.5));
#4192=DIRECTION('ref_axis',(0.5,0.,-0.866025403784439));
#4193=DIRECTION('center_axis',(0.,0.,-1.));
#4194=DIRECTION('ref_axis',(0.707106781186563,-0.707106781186532,0.));
#4195=DIRECTION('center_axis',(-2.54091264057109E-15,0.866025403784439,
-0.5));
#4196=DIRECTION('ref_axis',(1.43032168209504E-15,-0.5,-0.866025403784439));
#4197=DIRECTION('',(0.,0.,-1.));
#4198=DIRECTION('center_axis',(-1.,-4.30300426108057E-14,0.));
#4199=DIRECTION('ref_axis',(-4.30300426108057E-14,1.,0.));
#4200=DIRECTION('center_axis',(-1.,-4.30300426108057E-14,0.));
#4201=DIRECTION('ref_axis',(0.,0.,-1.));
#4202=DIRECTION('',(-2.15150213054029E-14,0.5,0.866025403784439));
#4203=DIRECTION('center_axis',(-2.54091264057109E-15,0.866025403784439,
-0.5));
#4204=DIRECTION('ref_axis',(1.,2.93399319404209E-15,0.));
#4205=DIRECTION('center_axis',(-2.54091264057109E-15,0.866025403784439,
-0.5));
#4206=DIRECTION('ref_axis',(0.,-0.5,-0.866025403784439));
#4207=DIRECTION('',(-1.,-2.93399319404209E-15,0.));
#4208=DIRECTION('center_axis',(-2.54091264057109E-15,0.866025403784439,
-0.5));
#4209=DIRECTION('ref_axis',(1.46699659702056E-15,-0.5,-0.866025403784439));
#4210=DIRECTION('',(-1.73044443434865E-14,-0.5,-0.866025403784439));
#4211=DIRECTION('center_axis',(1.,-3.4608888686973E-14,0.));
#4212=DIRECTION('ref_axis',(-3.4608888686973E-14,-1.,0.));
#4213=DIRECTION('center_axis',(1.,-3.4608888686973E-14,0.));
#4214=DIRECTION('ref_axis',(0.,0.,1.));
#4215=DIRECTION('',(0.,0.,1.));
#4216=DIRECTION('center_axis',(0.,0.,-1.));
#4217=DIRECTION('ref_axis',(-0.707106781186546,-0.707106781186549,0.));
#4218=DIRECTION('center_axis',(0.,0.,-1.));
#4219=DIRECTION('ref_axis',(-0.707106781186546,-0.707106781186549,0.));
#4220=DIRECTION('center_axis',(0.866025403784439,0.,-0.5));
#4221=DIRECTION('ref_axis',(-0.5,-3.66749149255139E-17,-0.866025403784439));
#4222=DIRECTION('',(0.,0.,-1.));
#4223=DIRECTION('center_axis',(-4.04626176340286E-14,1.,0.));
#4224=DIRECTION('ref_axis',(1.,4.04626176340286E-14,0.));
#4225=DIRECTION('center_axis',(-4.04626176340286E-14,1.,0.));
#4226=DIRECTION('ref_axis',(0.,0.,-1.));
#4227=DIRECTION('',(0.5,2.02313088170143E-14,0.866025403784439));
#4228=DIRECTION('center_axis',(0.866025403784439,0.,-0.5));
#4229=DIRECTION('ref_axis',(0.,-1.,0.));
#4230=DIRECTION('center_axis',(0.866025403784439,0.,-0.5));
#4231=DIRECTION('ref_axis',(0.5,0.,0.866025403784439));
#4232=DIRECTION('',(0.,1.,0.));
#4233=DIRECTION('center_axis',(0.866025403784439,0.,-0.5));
#4234=DIRECTION('ref_axis',(-0.5,3.66749149255139E-17,-0.866025403784439));
#4235=DIRECTION('',(-0.5,2.39626331165986E-16,-0.866025403784439));
#4236=DIRECTION('center_axis',(-4.79252662331972E-16,-1.,0.));
#4237=DIRECTION('ref_axis',(-1.,4.79252662331972E-16,0.));
#4238=DIRECTION('center_axis',(-4.79252662331972E-16,-1.,0.));
#4239=DIRECTION('ref_axis',(0.,0.,1.));
#4240=DIRECTION('',(0.,0.,1.));
#4241=DIRECTION('center_axis',(0.,0.,-1.));
#4242=DIRECTION('ref_axis',(0.70710678118653,0.707106781186565,0.));
#4243=DIRECTION('',(0.,0.,1.));
#4244=DIRECTION('center_axis',(-1.27045632028555E-15,-0.866025403784439,
-0.5));
#4245=DIRECTION('ref_axis',(6.96823383584764E-16,0.5,-0.866025403784439));
#4246=DIRECTION('center_axis',(0.,0.,-1.));
#4247=DIRECTION('ref_axis',(0.70710678118653,0.707106781186565,0.));
#4248=DIRECTION('center_axis',(-0.866025403784439,0.,-0.5));
#4249=DIRECTION('ref_axis',(0.5,3.66749149255139E-17,-0.866025403784439));
#4250=DIRECTION('',(0.,0.,-1.));
#4251=DIRECTION('center_axis',(5.35736011821097E-14,-1.,0.));
#4252=DIRECTION('ref_axis',(-1.,-5.35736011821097E-14,0.));
#4253=DIRECTION('center_axis',(5.35736011821097E-14,-1.,0.));
#4254=DIRECTION('ref_axis',(0.,0.,1.));
#4255=DIRECTION('',(-0.5,-2.67868005910549E-14,0.866025403784439));
#4256=DIRECTION('center_axis',(0.,0.,-1.));
#4257=DIRECTION('ref_axis',(-0.707106781186557,0.707106781186538,0.));
#4258=DIRECTION('center_axis',(0.,0.,-1.));
#4259=DIRECTION('ref_axis',(-0.707106781186557,0.707106781186538,0.));
#4260=DIRECTION('center_axis',(-1.27045632028555E-15,-0.866025403784439,
-0.5));
#4261=DIRECTION('ref_axis',(7.33498298510278E-16,0.5,-0.866025403784439));
#4262=DIRECTION('',(0.,0.,-1.));
#4263=DIRECTION('center_axis',(1.,2.81047454124667E-14,0.));
#4264=DIRECTION('ref_axis',(2.81047454124667E-14,-1.,0.));
#4265=DIRECTION('center_axis',(1.,2.81047454124667E-14,0.));
#4266=DIRECTION('ref_axis',(0.,0.,1.));
#4267=DIRECTION('',(1.40523727062334E-14,-0.5,0.866025403784439));
#4268=DIRECTION('center_axis',(0.,1.,0.));
#4269=DIRECTION('ref_axis',(1.,0.,0.));
#4270=DIRECTION('center_axis',(0.,1.,0.));
#4271=DIRECTION('ref_axis',(0.,0.,-1.));
#4272=DIRECTION('',(0.5,0.,-0.866025403784439));
#4273=DIRECTION('center_axis',(-0.866025403784439,0.,-0.5));
#4274=DIRECTION('ref_axis',(0.,1.,0.));
#4275=DIRECTION('center_axis',(-0.866025403784439,0.,-0.5));
#4276=DIRECTION('ref_axis',(0.5,0.,-0.866025403784439));
#4277=DIRECTION('',(0.,-1.,0.));
#4278=DIRECTION('center_axis',(-0.866025403784439,0.,-0.5));
#4279=DIRECTION('ref_axis',(0.5,0.,-0.866025403784439));
#4280=DIRECTION('center_axis',(-1.,3.8682536316795E-15,0.));
#4281=DIRECTION('ref_axis',(3.8682536316795E-15,1.,0.));
#4282=DIRECTION('center_axis',(-1.,3.8682536316795E-15,0.));
#4283=DIRECTION('ref_axis',(0.,0.,-1.));
#4284=DIRECTION('',(1.93412681583975E-15,0.5,-0.866025403784439));
#4285=DIRECTION('center_axis',(-1.27045632028555E-15,-0.866025403784439,
-0.5));
#4286=DIRECTION('ref_axis',(-1.,1.46699659702105E-15,0.));
#4287=DIRECTION('center_axis',(-1.27045632028555E-15,-0.866025403784439,
-0.5));
#4288=DIRECTION('ref_axis',(0.,-0.5,0.866025403784439));
#4289=DIRECTION('',(1.,-1.46699659702105E-15,0.));
#4290=DIRECTION('center_axis',(0.,0.,-1.));
#4291=DIRECTION('ref_axis',(-1.,0.,0.));
#4292=DIRECTION('center_axis',(0.,0.,-1.));
#4293=DIRECTION('ref_axis',(-1.,0.,0.));
#4294=DIRECTION('center_axis',(0.,0.,-1.));
#4295=DIRECTION('ref_axis',(1.,0.,0.));
#4296=DIRECTION('center_axis',(-1.22464679914735E-16,-1.,0.));
#4297=DIRECTION('ref_axis',(1.,-1.22464679914735E-16,0.));
#4298=DIRECTION('center_axis',(0.,0.,1.));
#4299=DIRECTION('ref_axis',(1.,0.,0.));
#4300=DIRECTION('center_axis',(0.,0.,-1.));
#4301=DIRECTION('ref_axis',(-1.,0.,0.));
#4302=DIRECTION('center_axis',(0.,0.,-1.));
#4303=DIRECTION('ref_axis',(1.,0.,0.));
#4304=DIRECTION('center_axis',(0.,0.,-1.));
#4305=DIRECTION('ref_axis',(-1.,0.,0.));
#4306=DIRECTION('center_axis',(0.,0.,-1.));
#4307=DIRECTION('ref_axis',(1.,0.,0.));
#4308=DIRECTION('',(0.,0.,1.));
#4309=DIRECTION('center_axis',(0.,0.,-1.));
#4310=DIRECTION('ref_axis',(-1.,0.,0.));
#4311=DIRECTION('center_axis',(0.,0.,-1.));
#4312=DIRECTION('ref_axis',(-1.,0.,0.));
#4313=DIRECTION('',(-0.258819045102519,3.16961915143174E-17,0.965925826289069));
#4314=DIRECTION('center_axis',(0.,0.,-1.));
#4315=DIRECTION('ref_axis',(-1.,0.,0.));
#4316=DIRECTION('center_axis',(0.,0.,1.));
#4317=DIRECTION('ref_axis',(-1.,0.,0.));
#4318=DIRECTION('',(0.,0.,1.));
#4319=DIRECTION('center_axis',(0.,0.,-1.));
#4320=DIRECTION('ref_axis',(-1.,0.,0.));
#4321=DIRECTION('center_axis',(6.12323399573676E-17,0.,1.));
#4322=DIRECTION('ref_axis',(1.,0.,0.));
#4323=DIRECTION('center_axis',(1.22464679914735E-16,-1.,0.));
#4324=DIRECTION('ref_axis',(-1.,-1.22464679914735E-16,0.));
#4325=DIRECTION('center_axis',(0.,0.,-1.));
#4326=DIRECTION('ref_axis',(1.,0.,0.));
#4327=DIRECTION('center_axis',(0.,0.,-1.));
#4328=DIRECTION('ref_axis',(1.,0.,0.));
#4329=DIRECTION('center_axis',(0.,0.,-1.));
#4330=DIRECTION('ref_axis',(-1.,0.,0.));
#4331=DIRECTION('',(-0.0871557427578718,1.06735001395738E-17,0.996194698090852));
#4332=DIRECTION('axis',(0.,0.,1.));
#4333=DIRECTION('refdir',(1.,0.,0.));
#4334=DIRECTION('center_axis',(0.,0.,-1.));
#4335=DIRECTION('ref_axis',(0.707106781186563,-0.707106781186532,0.));
#4336=DIRECTION('',(0.,0.,1.));
#4337=DIRECTION('center_axis',(-0.866025403784439,0.,-0.5));
#4338=DIRECTION('ref_axis',(0.5,0.,-0.866025403784439));
#4339=DIRECTION('center_axis',(0.,0.,-1.));
#4340=DIRECTION('ref_axis',(0.707106781186563,-0.707106781186532,0.));
#4341=DIRECTION('center_axis',(-2.54091264057109E-15,0.866025403784439,
-0.5));
#4342=DIRECTION('ref_axis',(1.43032168209504E-15,-0.5,-0.866025403784439));
#4343=DIRECTION('',(0.,0.,-1.));
#4344=DIRECTION('center_axis',(-1.,-4.30300426108057E-14,0.));
#4345=DIRECTION('ref_axis',(-4.30300426108057E-14,1.,0.));
#4346=DIRECTION('center_axis',(-1.,-4.30300426108057E-14,0.));
#4347=DIRECTION('ref_axis',(0.,0.,-1.));
#4348=DIRECTION('',(-2.15150213054029E-14,0.5,0.866025403784439));
#4349=DIRECTION('center_axis',(-2.54091264057109E-15,0.866025403784439,
-0.5));
#4350=DIRECTION('ref_axis',(1.,2.93399319404209E-15,0.));
#4351=DIRECTION('center_axis',(-2.54091264057109E-15,0.866025403784439,
-0.5));
#4352=DIRECTION('ref_axis',(0.,-0.5,-0.866025403784439));
#4353=DIRECTION('',(-1.,-2.93399319404209E-15,0.));
#4354=DIRECTION('center_axis',(-2.54091264057109E-15,0.866025403784439,
-0.5));
#4355=DIRECTION('ref_axis',(1.46699659702056E-15,-0.5,-0.866025403784439));
#4356=DIRECTION('',(-1.73044443434865E-14,-0.5,-0.866025403784439));
#4357=DIRECTION('center_axis',(1.,-3.4608888686973E-14,0.));
#4358=DIRECTION('ref_axis',(-3.4608888686973E-14,-1.,0.));
#4359=DIRECTION('center_axis',(1.,-3.4608888686973E-14,0.));
#4360=DIRECTION('ref_axis',(0.,0.,1.));
#4361=DIRECTION('',(0.,0.,1.));
#4362=DIRECTION('center_axis',(0.,0.,-1.));
#4363=DIRECTION('ref_axis',(-0.707106781186546,-0.707106781186549,0.));
#4364=DIRECTION('center_axis',(0.,0.,-1.));
#4365=DIRECTION('ref_axis',(-0.707106781186546,-0.707106781186549,0.));
#4366=DIRECTION('center_axis',(0.866025403784439,0.,-0.5));
#4367=DIRECTION('ref_axis',(-0.5,-3.66749149255139E-17,-0.866025403784439));
#4368=DIRECTION('',(0.,0.,-1.));
#4369=DIRECTION('center_axis',(-4.04626176340286E-14,1.,0.));
#4370=DIRECTION('ref_axis',(1.,4.04626176340286E-14,0.));
#4371=DIRECTION('center_axis',(-4.04626176340286E-14,1.,0.));
#4372=DIRECTION('ref_axis',(0.,0.,-1.));
#4373=DIRECTION('',(0.5,2.02313088170143E-14,0.866025403784439));
#4374=DIRECTION('center_axis',(0.866025403784439,0.,-0.5));
#4375=DIRECTION('ref_axis',(0.,-1.,0.));
#4376=DIRECTION('center_axis',(0.866025403784439,0.,-0.5));
#4377=DIRECTION('ref_axis',(0.5,0.,0.866025403784439));
#4378=DIRECTION('',(0.,1.,0.));
#4379=DIRECTION('center_axis',(0.866025403784439,0.,-0.5));
#4380=DIRECTION('ref_axis',(-0.5,3.66749149255139E-17,-0.866025403784439));
#4381=DIRECTION('',(-0.5,2.39626331165986E-16,-0.866025403784439));
#4382=DIRECTION('center_axis',(-4.79252662331972E-16,-1.,0.));
#4383=DIRECTION('ref_axis',(-1.,4.79252662331972E-16,0.));
#4384=DIRECTION('center_axis',(-4.79252662331972E-16,-1.,0.));
#4385=DIRECTION('ref_axis',(0.,0.,1.));
#4386=DIRECTION('',(0.,0.,1.));
#4387=DIRECTION('center_axis',(0.,0.,-1.));
#4388=DIRECTION('ref_axis',(0.70710678118653,0.707106781186565,0.));
#4389=DIRECTION('',(0.,0.,1.));
#4390=DIRECTION('center_axis',(-1.27045632028555E-15,-0.866025403784439,
-0.5));
#4391=DIRECTION('ref_axis',(6.96823383584764E-16,0.5,-0.866025403784439));
#4392=DIRECTION('center_axis',(0.,0.,-1.));
#4393=DIRECTION('ref_axis',(0.70710678118653,0.707106781186565,0.));
#4394=DIRECTION('center_axis',(-0.866025403784439,0.,-0.5));
#4395=DIRECTION('ref_axis',(0.5,3.66749149255139E-17,-0.866025403784439));
#4396=DIRECTION('',(0.,0.,-1.));
#4397=DIRECTION('center_axis',(5.35736011821097E-14,-1.,0.));
#4398=DIRECTION('ref_axis',(-1.,-5.35736011821097E-14,0.));
#4399=DIRECTION('center_axis',(5.35736011821097E-14,-1.,0.));
#4400=DIRECTION('ref_axis',(0.,0.,1.));
#4401=DIRECTION('',(-0.5,-2.67868005910549E-14,0.866025403784439));
#4402=DIRECTION('center_axis',(0.,0.,-1.));
#4403=DIRECTION('ref_axis',(-0.707106781186557,0.707106781186538,0.));
#4404=DIRECTION('center_axis',(0.,0.,-1.));
#4405=DIRECTION('ref_axis',(-0.707106781186557,0.707106781186538,0.));
#4406=DIRECTION('center_axis',(-1.27045632028555E-15,-0.866025403784439,
-0.5));
#4407=DIRECTION('ref_axis',(7.33498298510278E-16,0.5,-0.866025403784439));
#4408=DIRECTION('',(0.,0.,-1.));
#4409=DIRECTION('center_axis',(1.,2.81047454124667E-14,0.));
#4410=DIRECTION('ref_axis',(2.81047454124667E-14,-1.,0.));
#4411=DIRECTION('center_axis',(1.,2.81047454124667E-14,0.));
#4412=DIRECTION('ref_axis',(0.,0.,1.));
#4413=DIRECTION('',(1.40523727062334E-14,-0.5,0.866025403784439));
#4414=DIRECTION('center_axis',(0.,1.,0.));
#4415=DIRECTION('ref_axis',(1.,0.,0.));
#4416=DIRECTION('center_axis',(0.,1.,0.));
#4417=DIRECTION('ref_axis',(0.,0.,-1.));
#4418=DIRECTION('',(0.5,0.,-0.866025403784439));
#4419=DIRECTION('center_axis',(-0.866025403784439,0.,-0.5));
#4420=DIRECTION('ref_axis',(0.,1.,0.));
#4421=DIRECTION('center_axis',(-0.866025403784439,0.,-0.5));
#4422=DIRECTION('ref_axis',(0.5,0.,-0.866025403784439));
#4423=DIRECTION('',(0.,-1.,0.));
#4424=DIRECTION('center_axis',(-0.866025403784439,0.,-0.5));
#4425=DIRECTION('ref_axis',(0.5,0.,-0.866025403784439));
#4426=DIRECTION('center_axis',(-1.,3.8682536316795E-15,0.));
#4427=DIRECTION('ref_axis',(3.8682536316795E-15,1.,0.));
#4428=DIRECTION('center_axis',(-1.,3.8682536316795E-15,0.));
#4429=DIRECTION('ref_axis',(0.,0.,-1.));
#4430=DIRECTION('',(1.93412681583975E-15,0.5,-0.866025403784439));
#4431=DIRECTION('center_axis',(-1.27045632028555E-15,-0.866025403784439,
-0.5));
#4432=DIRECTION('ref_axis',(-1.,1.46699659702105E-15,0.));
#4433=DIRECTION('center_axis',(-1.27045632028555E-15,-0.866025403784439,
-0.5));
#4434=DIRECTION('ref_axis',(0.,-0.5,0.866025403784439));
#4435=DIRECTION('',(1.,-1.46699659702105E-15,0.));
#4436=DIRECTION('center_axis',(0.,0.,-1.));
#4437=DIRECTION('ref_axis',(-1.,0.,0.));
#4438=DIRECTION('center_axis',(0.,0.,-1.));
#4439=DIRECTION('ref_axis',(-1.,0.,0.));
#4440=DIRECTION('center_axis',(0.,0.,-1.));
#4441=DIRECTION('ref_axis',(1.,0.,0.));
#4442=DIRECTION('center_axis',(-1.22464679914735E-16,-1.,0.));
#4443=DIRECTION('ref_axis',(1.,-1.22464679914735E-16,0.));
#4444=DIRECTION('center_axis',(0.,0.,1.));
#4445=DIRECTION('ref_axis',(1.,0.,0.));
#4446=DIRECTION('center_axis',(0.,0.,-1.));
#4447=DIRECTION('ref_axis',(-1.,0.,0.));
#4448=DIRECTION('center_axis',(0.,0.,-1.));
#4449=DIRECTION('ref_axis',(1.,0.,0.));
#4450=DIRECTION('center_axis',(0.,0.,-1.));
#4451=DIRECTION('ref_axis',(-1.,0.,0.));
#4452=DIRECTION('center_axis',(0.,0.,-1.));
#4453=DIRECTION('ref_axis',(1.,0.,0.));
#4454=DIRECTION('',(0.,0.,1.));
#4455=DIRECTION('center_axis',(0.,0.,-1.));
#4456=DIRECTION('ref_axis',(-1.,0.,0.));
#4457=DIRECTION('center_axis',(0.,0.,-1.));
#4458=DIRECTION('ref_axis',(-1.,0.,0.));
#4459=DIRECTION('',(-0.258819045102519,3.16961915143174E-17,0.965925826289069));
#4460=DIRECTION('center_axis',(0.,0.,-1.));
#4461=DIRECTION('ref_axis',(-1.,0.,0.));
#4462=DIRECTION('center_axis',(0.,0.,1.));
#4463=DIRECTION('ref_axis',(-1.,0.,0.));
#4464=DIRECTION('',(0.,0.,1.));
#4465=DIRECTION('center_axis',(0.,0.,-1.));
#4466=DIRECTION('ref_axis',(-1.,0.,0.));
#4467=DIRECTION('center_axis',(6.12323399573676E-17,0.,1.));
#4468=DIRECTION('ref_axis',(1.,0.,0.));
#4469=DIRECTION('center_axis',(1.22464679914735E-16,-1.,0.));
#4470=DIRECTION('ref_axis',(-1.,-1.22464679914735E-16,0.));
#4471=DIRECTION('center_axis',(0.,0.,-1.));
#4472=DIRECTION('ref_axis',(1.,0.,0.));
#4473=DIRECTION('center_axis',(0.,0.,-1.));
#4474=DIRECTION('ref_axis',(1.,0.,0.));
#4475=DIRECTION('center_axis',(0.,0.,-1.));
#4476=DIRECTION('ref_axis',(-1.,0.,0.));
#4477=DIRECTION('',(-0.0871557427578718,1.06735001395738E-17,0.996194698090852));
#4478=DIRECTION('axis',(0.,0.,1.));
#4479=DIRECTION('refdir',(1.,0.,0.));
#4480=DIRECTION('center_axis',(0.,-1.,0.));
#4481=DIRECTION('ref_axis',(0.,0.,-1.));
#4482=DIRECTION('',(0.,0.,1.));
#4483=DIRECTION('',(-1.,0.,0.));
#4484=DIRECTION('',(0.,0.,-1.));
#4485=DIRECTION('',(1.,0.,0.));
#4486=DIRECTION('center_axis',(0.,0.,-1.));
#4487=DIRECTION('ref_axis',(0.,1.,0.));
#4488=DIRECTION('',(0.,-1.,0.));
#4489=DIRECTION('',(0.,1.,0.));
#4490=DIRECTION('',(1.,0.,0.));
#4491=DIRECTION('center_axis',(0.,1.,0.));
#4492=DIRECTION('ref_axis',(0.,0.,1.));
#4493=DIRECTION('',(0.,0.,-1.));
#4494=DIRECTION('',(0.,0.,1.));
#4495=DIRECTION('',(1.,0.,0.));
#4496=DIRECTION('center_axis',(-1.,0.,0.));
#4497=DIRECTION('ref_axis',(0.,0.,1.));
#4498=DIRECTION('',(0.,1.,0.));
#4499=DIRECTION('center_axis',(0.,0.,1.));
#4500=DIRECTION('ref_axis',(1.,0.,0.));
#4501=DIRECTION('',(0.,1.,0.));
#4502=DIRECTION('',(1.,0.,0.));
#4503=DIRECTION('',(0.,-1.,0.));
#4504=DIRECTION('',(-1.,0.,0.));
#4505=DIRECTION('',(0.,1.,0.));
#4506=DIRECTION('center_axis',(0.,0.,-1.));
#4507=DIRECTION('ref_axis',(-1.,0.,0.));
#4508=DIRECTION('center_axis',(0.,0.,-1.));
#4509=DIRECTION('ref_axis',(-1.,0.,0.));
#4510=DIRECTION('center_axis',(1.,0.,0.));
#4511=DIRECTION('ref_axis',(0.,-1.,0.));
#4512=DIRECTION('',(0.,0.,-1.));
#4513=DIRECTION('',(0.,-1.,0.));
#4514=DIRECTION('',(0.,0.,1.));
#4515=DIRECTION('center_axis',(0.,0.,1.));
#4516=DIRECTION('ref_axis',(1.,0.,0.));
#4517=DIRECTION('',(1.,0.,0.));
#4518=DIRECTION('',(0.,1.,0.));
#4519=DIRECTION('',(-1.,0.,0.));
#4520=DIRECTION('center_axis',(0.,0.,-1.));
#4521=DIRECTION('ref_axis',(-1.,0.,0.));
#4522=DIRECTION('center_axis',(0.,0.,-1.));
#4523=DIRECTION('ref_axis',(-1.,0.,0.));
#4524=DIRECTION('center_axis',(0.,-1.,0.));
#4525=DIRECTION('ref_axis',(1.,0.,0.));
#4526=DIRECTION('',(0.,0.,1.));
#4527=DIRECTION('center_axis',(0.,1.,0.));
#4528=DIRECTION('ref_axis',(-1.,0.,0.));
#4529=DIRECTION('',(0.,0.,1.));
#4530=DIRECTION('center_axis',(0.,0.,1.));
#4531=DIRECTION('ref_axis',(-1.,0.,0.));
#4532=DIRECTION('',(0.,0.,-1.));
#4533=DIRECTION('center_axis',(0.,0.,-1.));
#4534=DIRECTION('ref_axis',(-1.,0.,0.));
#4535=DIRECTION('',(0.,0.,-1.));
#4536=DIRECTION('center_axis',(1.,0.,0.));
#4537=DIRECTION('ref_axis',(0.,1.,0.));
#4538=DIRECTION('axis',(0.,0.,1.));
#4539=DIRECTION('refdir',(1.,0.,0.));
#4540=DIRECTION('center_axis',(0.,1.,0.));
#4541=DIRECTION('ref_axis',(0.,0.,-1.));
#4542=DIRECTION('',(0.,0.,1.));
#4543=DIRECTION('',(-1.,0.,0.));
#4544=DIRECTION('',(0.,0.,-1.));
#4545=DIRECTION('',(-1.,0.,0.));
#4546=DIRECTION('center_axis',(0.,0.,1.));
#4547=DIRECTION('ref_axis',(0.,1.,0.));
#4548=DIRECTION('',(0.,-1.,0.));
#4549=DIRECTION('',(0.,1.,0.));
#4550=DIRECTION('',(-1.,0.,0.));
#4551=DIRECTION('center_axis',(0.,-1.,0.));
#4552=DIRECTION('ref_axis',(0.,0.,1.));
#4553=DIRECTION('',(0.,0.,-1.));
#4554=DIRECTION('',(0.,0.,1.));
#4555=DIRECTION('',(-1.,0.,0.));
#4556=DIRECTION('center_axis',(-1.,0.,0.));
#4557=DIRECTION('ref_axis',(0.,0.,1.));
#4558=DIRECTION('',(0.,-1.,0.));
#4559=DIRECTION('center_axis',(1.,0.,0.));
#4560=DIRECTION('ref_axis',(0.,-1.,0.));
#4561=DIRECTION('',(0.,1.,0.));
#4562=DIRECTION('',(0.,0.,-1.));
#4563=DIRECTION('',(0.,-1.,0.));
#4564=DIRECTION('',(0.,0.,1.));
#4565=DIRECTION('',(0.,1.,0.));
#4566=DIRECTION('center_axis',(0.,1.,0.));
#4567=DIRECTION('ref_axis',(1.,0.,0.));
#4568=DIRECTION('center_axis',(0.,1.,0.));
#4569=DIRECTION('ref_axis',(1.,0.,0.));
#4570=DIRECTION('',(0.,1.,0.));
#4571=DIRECTION('center_axis',(0.,-1.,0.));
#4572=DIRECTION('ref_axis',(1.,0.,0.));
#4573=DIRECTION('center_axis',(0.,-1.,0.));
#4574=DIRECTION('ref_axis',(-1.,0.,0.));
#4575=DIRECTION('',(1.,0.,0.));
#4576=DIRECTION('',(0.,0.,-1.));
#4577=DIRECTION('',(-1.,0.,0.));
#4578=DIRECTION('',(0.,0.,1.));
#4579=DIRECTION('center_axis',(0.,1.,0.));
#4580=DIRECTION('ref_axis',(1.,0.,0.));
#4581=DIRECTION('',(-1.,0.,0.));
#4582=DIRECTION('',(0.,0.,-1.));
#4583=DIRECTION('',(1.,0.,0.));
#4584=DIRECTION('',(0.,0.,-1.));
#4585=DIRECTION('center_axis',(-1.,0.,0.));
#4586=DIRECTION('ref_axis',(0.,1.,0.));
#4587=DIRECTION('',(0.,-1.,0.));
#4588=DIRECTION('',(0.,1.,0.));
#4589=DIRECTION('center_axis',(-1.,0.,0.));
#4590=DIRECTION('ref_axis',(0.,1.,0.));
#4591=DIRECTION('',(0.,1.,0.));
#4592=DIRECTION('',(0.,0.,-1.));
#4593=DIRECTION('',(0.,-1.,0.));
#4594=DIRECTION('',(0.,0.,-1.));
#4595=DIRECTION('',(0.,-1.,0.));
#4596=DIRECTION('center_axis',(0.,-1.,0.));
#4597=DIRECTION('ref_axis',(-1.,0.,0.));
#4598=DIRECTION('',(0.,0.,1.));
#4599=DIRECTION('',(-1.,0.,0.));
#4600=DIRECTION('',(0.,0.,-1.));
#4601=DIRECTION('',(-1.,0.,0.));
#4602=DIRECTION('center_axis',(0.,1.,0.));
#4603=DIRECTION('ref_axis',(1.,0.,0.));
#4604=DIRECTION('',(1.,0.,0.));
#4605=DIRECTION('',(0.,0.,-1.));
#4606=DIRECTION('',(1.,0.,0.));
#4607=DIRECTION('center_axis',(-1.,0.,0.));
#4608=DIRECTION('ref_axis',(0.,1.,0.));
#4609=DIRECTION('',(0.,1.,0.));
#4610=DIRECTION('',(0.,1.,0.));
#4611=DIRECTION('center_axis',(0.,0.,-1.));
#4612=DIRECTION('ref_axis',(-1.,0.,0.));
#4613=DIRECTION('center_axis',(0.,0.,1.));
#4614=DIRECTION('ref_axis',(-1.,8.88178419700126E-16,0.));
#4615=DIRECTION('center_axis',(0.,1.,0.));
#4616=DIRECTION('ref_axis',(1.,0.,0.));
#4617=DIRECTION('',(1.,0.,0.));
#4618=DIRECTION('',(0.,0.,-1.));
#4619=DIRECTION('',(-1.,0.,0.));
#4620=DIRECTION('',(0.,0.,-1.));
#4621=DIRECTION('center_axis',(0.,0.,-1.));
#4622=DIRECTION('ref_axis',(1.33226762955019E-15,1.,0.));
#4623=DIRECTION('center_axis',(0.,0.,1.));
#4624=DIRECTION('ref_axis',(1.33226762955019E-15,1.,0.));
#4625=DIRECTION('center_axis',(0.,0.,-1.));
#4626=DIRECTION('ref_axis',(1.33226762955019E-15,1.,0.));
#4627=DIRECTION('center_axis',(0.,1.,0.));
#4628=DIRECTION('ref_axis',(-1.,0.,0.));
#4629=DIRECTION('',(0.,0.,-1.));
#4630=DIRECTION('',(1.,0.,0.));
#4631=DIRECTION('',(-1.,0.,0.));
#4632=DIRECTION('center_axis',(0.,0.,1.));
#4633=DIRECTION('ref_axis',(1.,0.,0.));
#4634=DIRECTION('',(0.,-1.,0.));
#4635=DIRECTION('',(-1.,0.,0.));
#4636=DIRECTION('',(0.,-1.,0.));
#4637=DIRECTION('center_axis',(0.,0.,1.));
#4638=DIRECTION('ref_axis',(-1.,8.88178419700126E-16,0.));
#4639=DIRECTION('center_axis',(-1.,0.,0.));
#4640=DIRECTION('ref_axis',(0.,1.,0.));
#4641=DIRECTION('',(0.,1.,0.));
#4642=DIRECTION('center_axis',(0.,0.,1.));
#4643=DIRECTION('ref_axis',(1.,0.,0.));
#4644=DIRECTION('',(0.,1.,0.));
#4645=DIRECTION('',(1.,0.,0.));
#4646=DIRECTION('center_axis',(0.,0.,-1.));
#4647=DIRECTION('ref_axis',(-1.,8.88178419700126E-16,0.));
#4648=DIRECTION('',(0.,0.,-1.));
#4649=DIRECTION('center_axis',(0.,-1.,0.));
#4650=DIRECTION('ref_axis',(1.,0.,0.));
#4651=DIRECTION('',(0.,0.,1.));
#4652=DIRECTION('center_axis',(-1.,0.,0.));
#4653=DIRECTION('ref_axis',(0.,1.,0.));
#4654=DIRECTION('axis',(0.,0.,1.));
#4655=DIRECTION('refdir',(1.,0.,0.));
#4656=DIRECTION('center_axis',(0.,-1.,0.));
#4657=DIRECTION('ref_axis',(0.,0.,1.));
#4658=DIRECTION('',(0.,0.,1.));
#4659=DIRECTION('',(1.,0.,0.));
#4660=DIRECTION('',(0.,0.,1.));
#4661=DIRECTION('',(-1.,0.,0.));
#4662=DIRECTION('center_axis',(0.,0.,1.));
#4663=DIRECTION('ref_axis',(0.,1.,0.));
#4664=DIRECTION('',(0.,1.,0.));
#4665=DIRECTION('',(0.,1.,0.));
#4666=DIRECTION('',(-1.,0.,0.));
#4667=DIRECTION('center_axis',(0.,1.,0.));
#4668=DIRECTION('ref_axis',(0.,0.,-1.));
#4669=DIRECTION('',(0.,0.,-1.));
#4670=DIRECTION('',(0.,0.,-1.));
#4671=DIRECTION('',(-1.,0.,0.));
#4672=DIRECTION('center_axis',(-1.,0.,0.));
#4673=DIRECTION('ref_axis',(0.,0.,1.));
#4674=DIRECTION('',(0.,-1.,0.));
#4675=DIRECTION('center_axis',(-1.,0.,0.));
#4676=DIRECTION('ref_axis',(0.,1.,0.));
#4677=DIRECTION('',(0.,-1.,0.));
#4678=DIRECTION('',(0.,0.,-1.));
#4679=DIRECTION('',(0.,1.,0.));
#4680=DIRECTION('',(0.,0.,1.));
#4681=DIRECTION('',(0.,-1.,0.));
#4682=DIRECTION('center_axis',(0.,0.,1.));
#4683=DIRECTION('ref_axis',(1.,0.,0.));
#4684=DIRECTION('',(-1.,0.,0.));
#4685=DIRECTION('',(0.,-1.,0.));
#4686=DIRECTION('',(1.,0.,0.));
#4687=DIRECTION('center_axis',(0.,0.,-1.));
#4688=DIRECTION('ref_axis',(1.,0.,0.));
#4689=DIRECTION('center_axis',(0.,0.,-1.));
#4690=DIRECTION('ref_axis',(1.,0.,0.));
#4691=DIRECTION('center_axis',(0.,-1.,0.));
#4692=DIRECTION('ref_axis',(1.,0.,0.));
#4693=DIRECTION('',(0.,0.,1.));
#4694=DIRECTION('',(-1.,0.,0.));
#4695=DIRECTION('center_axis',(0.,0.,1.));
#4696=DIRECTION('ref_axis',(1.,0.,0.));
#4697=DIRECTION('',(0.,1.,0.));
#4698=DIRECTION('',(1.,0.,0.));
#4699=DIRECTION('center_axis',(0.,0.,-1.));
#4700=DIRECTION('ref_axis',(1.,0.,0.));
#4701=DIRECTION('center_axis',(0.,0.,-1.));
#4702=DIRECTION('ref_axis',(1.,0.,0.));
#4703=DIRECTION('center_axis',(0.,1.,0.));
#4704=DIRECTION('ref_axis',(-1.,0.,0.));
#4705=DIRECTION('',(0.,0.,1.));
#4706=DIRECTION('center_axis',(0.,0.,-1.));
#4707=DIRECTION('ref_axis',(1.,0.,0.));
#4708=DIRECTION('',(0.,0.,-1.));
#4709=DIRECTION('center_axis',(0.,0.,1.));
#4710=DIRECTION('ref_axis',(1.,0.,0.));
#4711=DIRECTION('',(0.,0.,-1.));
#4712=DIRECTION('center_axis',(-1.,0.,0.));
#4713=DIRECTION('ref_axis',(0.,-1.,0.));
#4714=DIRECTION('axis',(0.,0.,1.));
#4715=DIRECTION('refdir',(1.,0.,0.));
#4716=DIRECTION('center_axis',(0.,-1.,0.));
#4717=DIRECTION('ref_axis',(0.,0.,-1.));
#4718=DIRECTION('',(0.,0.,-1.));
#4719=DIRECTION('',(1.,0.,0.));
#4720=DIRECTION('',(0.,0.,-1.));
#4721=DIRECTION('',(1.,0.,0.));
#4722=DIRECTION('center_axis',(0.,0.,-1.));
#4723=DIRECTION('ref_axis',(0.,1.,0.));
#4724=DIRECTION('',(0.,1.,0.));
#4725=DIRECTION('',(1.,0.,0.));
#4726=DIRECTION('',(0.,1.,0.));
#4727=DIRECTION('center_axis',(0.,1.,0.));
#4728=DIRECTION('ref_axis',(0.,0.,1.));
#4729=DIRECTION('',(0.,0.,1.));
#4730=DIRECTION('',(1.,0.,0.));
#4731=DIRECTION('',(0.,0.,1.));
#4732=DIRECTION('center_axis',(-1.,0.,0.));
#4733=DIRECTION('ref_axis',(0.,0.,1.));
#4734=DIRECTION('',(0.,-1.,0.));
#4735=DIRECTION('center_axis',(-1.,0.,0.));
#4736=DIRECTION('ref_axis',(0.,1.,0.));
#4737=DIRECTION('',(0.,-1.,0.));
#4738=DIRECTION('',(0.,0.,1.));
#4739=DIRECTION('',(0.,1.,0.));
#4740=DIRECTION('',(0.,0.,1.));
#4741=DIRECTION('',(0.,-1.,0.));
#4742=DIRECTION('center_axis',(1.,0.,0.));
#4743=DIRECTION('ref_axis',(0.,-1.,0.));
#4744=DIRECTION('',(0.,1.,0.));
#4745=DIRECTION('',(0.,0.,-1.));
#4746=DIRECTION('',(0.,-1.,0.));
#4747=DIRECTION('',(0.,0.,1.));
#4748=DIRECTION('center_axis',(0.,-1.,0.));
#4749=DIRECTION('ref_axis',(-1.,0.,0.));
#4750=DIRECTION('',(1.,0.,0.));
#4751=DIRECTION('',(0.,0.,-1.));
#4752=DIRECTION('',(-1.,0.,0.));
#4753=DIRECTION('center_axis',(0.,0.,-1.));
#4754=DIRECTION('ref_axis',(-1.,8.88178419700126E-16,0.));
#4755=DIRECTION('center_axis',(0.,0.,-1.));
#4756=DIRECTION('ref_axis',(-1.,8.88178419700126E-16,0.));
#4757=DIRECTION('',(0.,0.,-1.));
#4758=DIRECTION('center_axis',(0.,0.,1.));
#4759=DIRECTION('ref_axis',(-1.,8.88178419700126E-16,0.));
#4760=DIRECTION('center_axis',(0.,0.,1.));
#4761=DIRECTION('ref_axis',(1.,0.,0.));
#4762=DIRECTION('',(1.,0.,0.));
#4763=DIRECTION('center_axis',(0.,0.,1.));
#4764=DIRECTION('ref_axis',(-1.33226762955019E-15,-1.,0.));
#4765=DIRECTION('',(0.,1.,0.));
#4766=DIRECTION('',(1.,0.,0.));
#4767=DIRECTION('',(0.,1.,0.));
#4768=DIRECTION('',(-1.,0.,0.));
#4769=DIRECTION('center_axis',(0.,0.,1.));
#4770=DIRECTION('ref_axis',(1.,-8.88178419700126E-16,0.));
#4771=DIRECTION('',(-1.,0.,0.));
#4772=DIRECTION('center_axis',(0.,-1.,0.));
#4773=DIRECTION('ref_axis',(-1.,0.,0.));
#4774=DIRECTION('',(-1.,0.,0.));
#4775=DIRECTION('',(0.,0.,-1.));
#4776=DIRECTION('center_axis',(0.,-1.,0.));
#4777=DIRECTION('ref_axis',(1.,0.,0.));
#4778=DIRECTION('center_axis',(1.,0.,0.));
#4779=DIRECTION('ref_axis',(0.,-1.,0.));
#4780=DIRECTION('',(0.,0.,-1.));
#4781=DIRECTION('',(0.,0.,-1.));
#4782=DIRECTION('',(0.,1.,0.));
#4783=DIRECTION('',(0.,0.,1.));
#4784=DIRECTION('',(0.,-1.,0.));
#4785=DIRECTION('center_axis',(0.,0.,-1.));
#4786=DIRECTION('ref_axis',(-1.33226762955019E-15,-1.,0.));
#4787=DIRECTION('',(0.,0.,-1.));
#4788=DIRECTION('center_axis',(0.,0.,1.));
#4789=DIRECTION('ref_axis',(-1.33226762955019E-15,-1.,0.));
#4790=DIRECTION('center_axis',(0.,0.,-1.));
#4791=DIRECTION('ref_axis',(-1.33226762955019E-15,-1.,0.));
#4792=DIRECTION('center_axis',(1.,0.,0.));
#4793=DIRECTION('ref_axis',(0.,-1.,0.));
#4794=DIRECTION('',(0.,-1.,0.));
#4795=DIRECTION('',(0.,0.,-1.));
#4796=DIRECTION('',(0.,-1.,0.));
#4797=DIRECTION('',(0.,0.,-1.));
#4798=DIRECTION('center_axis',(0.,1.,0.));
#4799=DIRECTION('ref_axis',(1.,0.,0.));
#4800=DIRECTION('',(1.,0.,0.));
#4801=DIRECTION('',(1.,0.,0.));
#4802=DIRECTION('center_axis',(0.,0.,-1.));
#4803=DIRECTION('ref_axis',(-1.,0.,0.));
#4804=DIRECTION('',(-1.,0.,0.));
#4805=DIRECTION('center_axis',(0.,-1.,0.));
#4806=DIRECTION('ref_axis',(-1.,0.,0.));
#4807=DIRECTION('',(-1.,0.,0.));
#4808=DIRECTION('center_axis',(0.,0.,-1.));
#4809=DIRECTION('ref_axis',(1.,-8.88178419700126E-16,0.));
#4810=DIRECTION('',(0.,0.,1.));
#4811=DIRECTION('center_axis',(0.,0.,-1.));
#4812=DIRECTION('ref_axis',(1.,-8.88178419700126E-16,0.));
#4813=DIRECTION('center_axis',(1.,0.,0.));
#4814=DIRECTION('ref_axis',(0.,-1.,0.));
#4815=DIRECTION('',(0.,0.,-1.));
#4816=DIRECTION('',(0.,-1.,0.));
#4817=DIRECTION('',(0.,0.,-1.));
#4818=DIRECTION('center_axis',(0.,-1.,0.));
#4819=DIRECTION('ref_axis',(-1.,0.,0.));
#4820=DIRECTION('',(-1.,0.,0.));
#4821=DIRECTION('center_axis',(0.,1.,0.));
#4822=DIRECTION('ref_axis',(1.,0.,0.));
#4823=DIRECTION('',(1.,0.,0.));
#4824=DIRECTION('center_axis',(0.,1.,0.));
#4825=DIRECTION('ref_axis',(1.,0.,0.));
#4826=DIRECTION('center_axis',(0.,1.,0.));
#4827=DIRECTION('ref_axis',(1.,0.,0.));
#4828=DIRECTION('',(0.,1.,0.));
#4829=DIRECTION('center_axis',(0.,-1.,0.));
#4830=DIRECTION('ref_axis',(1.,0.,0.));
#4831=DIRECTION('',(1.,0.,0.));
#4832=DIRECTION('center_axis',(0.,0.,1.));
#4833=DIRECTION('ref_axis',(1.,0.,0.));
#4834=DIRECTION('axis',(0.,0.,1.));
#4835=DIRECTION('refdir',(1.,0.,0.));
#4836=DIRECTION('center_axis',(0.,0.,1.));
#4837=DIRECTION('ref_axis',(1.,0.,0.));
#4838=DIRECTION('center_axis',(0.,1.46957615897682E-15,1.));
#4839=DIRECTION('ref_axis',(1.,0.,0.));
#4840=DIRECTION('center_axis',(0.,1.46957615897682E-15,1.));
#4841=DIRECTION('ref_axis',(1.,0.,0.));
#4842=DIRECTION('center_axis',(0.,0.,1.));
#4843=DIRECTION('ref_axis',(1.,0.,0.));
#4844=DIRECTION('axis',(0.,0.,1.));
#4845=DIRECTION('refdir',(1.,0.,0.));
#4846=DIRECTION('center_axis',(0.,1.,0.));
#4847=DIRECTION('ref_axis',(1.,0.,0.));
#4848=DIRECTION('',(1.,0.,0.));
#4849=DIRECTION('',(0.,0.,-1.));
#4850=DIRECTION('',(1.,0.,0.));
#4851=DIRECTION('',(0.,0.,-1.));
#4852=DIRECTION('center_axis',(1.,-1.03276560430247E-15,0.));
#4853=DIRECTION('ref_axis',(-1.03276560430247E-15,-1.,0.));
#4854=DIRECTION('',(-1.03276560430247E-15,-1.,0.));
#4855=DIRECTION('',(0.,0.,-1.));
#4856=DIRECTION('',(-1.03276560430247E-15,-1.,0.));
#4857=DIRECTION('center_axis',(0.,-1.,0.));
#4858=DIRECTION('ref_axis',(-1.,0.,0.));
#4859=DIRECTION('',(-1.,0.,0.));
#4860=DIRECTION('',(0.,0.,-1.));
#4861=DIRECTION('',(-1.,0.,0.));
#4862=DIRECTION('center_axis',(-1.,1.03276560430247E-15,0.));
#4863=DIRECTION('ref_axis',(1.03276560430247E-15,1.,0.));
#4864=DIRECTION('',(1.03276560430247E-15,1.,0.));
#4865=DIRECTION('',(1.03276560430247E-15,1.,0.));
#4866=DIRECTION('center_axis',(0.,0.,-1.));
#4867=DIRECTION('ref_axis',(-1.,0.,0.));
#4868=DIRECTION('',(1.,0.,0.));
#4869=DIRECTION('',(0.,1.,0.));
#4870=DIRECTION('',(-1.,0.,0.));
#4871=DIRECTION('',(0.,-1.,0.));
#4872=DIRECTION('center_axis',(-1.,0.,0.));
#4873=DIRECTION('ref_axis',(0.,1.,0.));
#4874=DIRECTION('',(0.,0.,-1.));
#4875=DIRECTION('',(0.,1.,0.));
#4876=DIRECTION('',(0.,0.,-1.));
#4877=DIRECTION('center_axis',(0.,1.,0.));
#4878=DIRECTION('ref_axis',(1.,0.,0.));
#4879=DIRECTION('',(0.,0.,-1.));
#4880=DIRECTION('',(1.,0.,0.));
#4881=DIRECTION('center_axis',(1.,0.,0.));
#4882=DIRECTION('ref_axis',(0.,-1.,0.));
#4883=DIRECTION('',(0.,-1.,0.));
#4884=DIRECTION('',(0.,0.,-1.));
#4885=DIRECTION('',(0.,-1.,0.));
#4886=DIRECTION('',(0.,0.,-1.));
#4887=DIRECTION('center_axis',(0.,1.,0.));
#4888=DIRECTION('ref_axis',(1.,0.,0.));
#4889=DIRECTION('',(1.,0.,0.));
#4890=DIRECTION('',(0.,0.,-1.));
#4891=DIRECTION('',(1.,0.,0.));
#4892=DIRECTION('center_axis',(-1.,0.,0.));
#4893=DIRECTION('ref_axis',(0.,1.,0.));
#4894=DIRECTION('',(0.,1.,0.));
#4895=DIRECTION('',(0.,0.,-1.));
#4896=DIRECTION('',(0.,1.,0.));
#4897=DIRECTION('center_axis',(0.,-1.,0.));
#4898=DIRECTION('ref_axis',(-1.,0.,0.));
#4899=DIRECTION('',(-1.,0.,0.));
#4900=DIRECTION('',(-1.,0.,0.));
#4901=DIRECTION('center_axis',(0.,0.,-1.));
#4902=DIRECTION('ref_axis',(-1.,0.,0.));
#4903=DIRECTION('center_axis',(0.,-1.,0.));
#4904=DIRECTION('ref_axis',(-1.,0.,0.));
#4905=DIRECTION('',(-1.,0.,0.));
#4906=DIRECTION('',(0.,0.,-1.));
#4907=DIRECTION('center_axis',(1.,0.,0.));
#4908=DIRECTION('ref_axis',(0.,-1.,0.));
#4909=DIRECTION('',(0.,-1.,0.));
#4910=DIRECTION('center_axis',(0.,0.,1.));
#4911=DIRECTION('ref_axis',(-1.,0.,0.));
#4912=DIRECTION('center_axis',(0.,0.,-1.));
#4913=DIRECTION('ref_axis',(-1.,0.,0.));
#4914=DIRECTION('',(0.,1.22464679914735E-16,1.));
#4915=DIRECTION('',(1.,0.,0.));
#4916=DIRECTION('',(0.,1.22464679914735E-16,1.));
#4917=DIRECTION('',(1.,0.,0.));
#4918=DIRECTION('',(0.,1.22464679914735E-16,1.));
#4919=DIRECTION('',(1.,0.,0.));
#4920=DIRECTION('',(0.,1.22464679914735E-16,1.));
#4921=DIRECTION('',(1.,0.,0.));
#4922=DIRECTION('',(0.,0.,1.));
#4923=DIRECTION('',(1.,0.,0.));
#4924=DIRECTION('',(0.,0.,1.));
#4925=DIRECTION('',(1.,0.,0.));
#4926=DIRECTION('',(0.,0.,1.));
#4927=DIRECTION('',(1.,0.,0.));
#4928=DIRECTION('',(0.,0.,1.));
#4929=DIRECTION('',(1.,0.,0.));
#4930=DIRECTION('',(0.,0.,1.));
#4931=DIRECTION('',(1.,0.,0.));
#4932=DIRECTION('',(0.,0.,1.));
#4933=DIRECTION('',(1.,0.,0.));
#4934=CARTESIAN_POINT('',(0.,0.,0.));
#4935=CARTESIAN_POINT('',(0.,0.,0.));
#4936=CARTESIAN_POINT('Origin',(-1.41899999999985,1.41899999999965,3.1));
#4937=CARTESIAN_POINT('',(-1.41899999999985,0.472999999999654,3.01252522110193));
#4938=CARTESIAN_POINT('',(-0.472999999999848,1.41899999999969,3.01252522110194));
#4939=CARTESIAN_POINT('Ctrl Pts',(-1.41899999999985,0.472999999999654,3.01252522110193));
#4940=CARTESIAN_POINT('Ctrl Pts',(-1.418237843063,0.472999999999654,3.01261008153857));
#4941=CARTESIAN_POINT('Ctrl Pts',(-1.41747599318127,0.473000921064105,3.01269480438576));
#4942=CARTESIAN_POINT('Ctrl Pts',(-1.29873656917598,0.473287797471327,3.02588334070707));
#4943=CARTESIAN_POINT('Ctrl Pts',(-1.17260477262757,0.497030428020145,3.03726209636997));
#4944=CARTESIAN_POINT('Ctrl Pts',(-0.940241249793281,0.593452559529333,
3.05235989856665));
#4945=CARTESIAN_POINT('Ctrl Pts',(-0.834013199901804,0.666140770092746,
3.05607990145755));
#4946=CARTESIAN_POINT('Ctrl Pts',(-0.75007698499736,0.750076984997194,3.05607990145756));
#4947=CARTESIAN_POINT('Ctrl Pts',(-0.666140770092915,0.834013199901643,
3.05607990145756));
#4948=CARTESIAN_POINT('Ctrl Pts',(-0.593452559529506,0.940241249793123,
3.05235989856665));
#4949=CARTESIAN_POINT('Ctrl Pts',(-0.497030428020328,1.17260477262741,3.03726209636997));
#4950=CARTESIAN_POINT('Ctrl Pts',(-0.473287797471517,1.29873656917583,3.02588334070708));
#4951=CARTESIAN_POINT('Ctrl Pts',(-0.4730009210643,1.41747599318095,3.01269480438579));
#4952=CARTESIAN_POINT('Ctrl Pts',(-0.472999999999848,1.41823784306269,3.0126100815386));
#4953=CARTESIAN_POINT('Ctrl Pts',(-0.472999999999848,1.41899999999969,3.01252522110194));
#4954=CARTESIAN_POINT('',(-1.41899999999985,0.472999999999654,1.22765307701778));
#4955=CARTESIAN_POINT('',(-1.41899999999985,0.472999999999654,3.1));
#4956=CARTESIAN_POINT('',(-0.866098738193358,0.651395808574938,0.27));
#4957=CARTESIAN_POINT('Origin',(-1.41899999999985,1.41899999999965,1.22765307701778));
#4958=CARTESIAN_POINT('',(-0.651395808574991,0.86609873819336,0.27));
#4959=CARTESIAN_POINT('Origin',(-1.41899999999985,1.41899999999965,0.27));
#4960=CARTESIAN_POINT('',(-0.472999999999848,1.41899999999969,1.22765307701751));
#4961=CARTESIAN_POINT('Origin',(-1.41899999999985,1.41899999999965,1.22765307701745));
#4962=CARTESIAN_POINT('',(-0.472999999999848,1.41899999999969,3.1));
#4963=CARTESIAN_POINT('Origin',(-0.472999999999807,0.472999999999754,3.1));
#4964=CARTESIAN_POINT('',(-0.472999999999889,2.36767196216383,2.87080111520185));
#4965=CARTESIAN_POINT('Origin',(-0.472999999999787,-2.0353210154902E-14,
-9.73193776093083));
#4966=CARTESIAN_POINT('',(-0.472999999999884,2.24662499999997,2.66114162663218));
#4967=CARTESIAN_POINT('Origin',(-0.472999999999895,2.5,3.1));
#4968=CARTESIAN_POINT('',(0.472999999999787,2.36767196216383,2.87080111520185));
#4969=CARTESIAN_POINT('Origin',(1.16338464595253E-14,-3.68139204037345,
-7.60648507542867));
#4970=CARTESIAN_POINT('',(0.651395808575038,0.866098738193364,0.27));
#4971=CARTESIAN_POINT('',(-0.236499999999946,0.866098738193362,0.27));
#4972=CARTESIAN_POINT('',(0.472999999999754,1.41899999999989,1.22765307701784));
#4973=CARTESIAN_POINT('Origin',(1.41899999999975,1.41899999999985,1.22765307701778));
#4974=CARTESIAN_POINT('',(0.472999999999791,2.5,3.09999999999999));
#4975=CARTESIAN_POINT('Origin',(0.472999999999791,2.5,3.1));
#4976=CARTESIAN_POINT('',(0.472999999999754,1.41899999999989,3.01252522110192));
#4977=CARTESIAN_POINT('Origin',(0.472999999999705,-1.6370004348928E-14,
-9.73193776093083));
#4978=CARTESIAN_POINT('',(0.472999999999754,1.41899999999989,3.1));
#4979=CARTESIAN_POINT('Origin',(1.41899999999975,1.41899999999985,3.1));
#4980=CARTESIAN_POINT('',(1.41899999999979,0.472999999999854,3.01252522110193));
#4981=CARTESIAN_POINT('Ctrl Pts',(0.472999999999754,1.41899999999989,3.01252522110192));
#4982=CARTESIAN_POINT('Ctrl Pts',(0.472999999999754,1.41823784306304,3.01261008153856));
#4983=CARTESIAN_POINT('Ctrl Pts',(0.473000921064206,1.4174759931813,3.01269480438575));
#4984=CARTESIAN_POINT('Ctrl Pts',(0.473287797471426,1.29873656917601,3.02588334070706));
#4985=CARTESIAN_POINT('Ctrl Pts',(0.49703042802024,1.17260477262759,3.03726209636996));
#4986=CARTESIAN_POINT('Ctrl Pts',(0.593452559529424,0.940241249793303,3.05235989856665));
#4987=CARTESIAN_POINT('Ctrl Pts',(0.666140770092836,0.834013199901824,3.05607990145755));
#4988=CARTESIAN_POINT('Ctrl Pts',(0.750076984997282,0.750076984997378,3.05607990145755));
#4989=CARTESIAN_POINT('Ctrl Pts',(0.834013199901729,0.666140770092932,3.05607990145755));
#4990=CARTESIAN_POINT('Ctrl Pts',(0.940241249793208,0.593452559529521,3.05235989856665));
#4991=CARTESIAN_POINT('Ctrl Pts',(1.1726047726275,0.497030428020338,3.03726209636996));
#4992=CARTESIAN_POINT('Ctrl Pts',(1.29873656917591,0.473287797471525,3.02588334070707));
#4993=CARTESIAN_POINT('Ctrl Pts',(1.41747599318104,0.473000921064306,3.01269480438578));
#4994=CARTESIAN_POINT('Ctrl Pts',(1.41823784306278,0.472999999999854,3.01261008153858));
#4995=CARTESIAN_POINT('Ctrl Pts',(1.41899999999979,0.472999999999854,3.01252522110193));
#4996=CARTESIAN_POINT('',(0.866098738193361,0.651395808575069,0.27));
#4997=CARTESIAN_POINT('Origin',(1.41899999999975,1.41899999999985,0.27));
#4998=CARTESIAN_POINT('',(1.41899999999979,0.472999999999853,1.22765307701768));
#4999=CARTESIAN_POINT('Origin',(1.41899999999975,1.41899999999985,1.22765307701762));
#5000=CARTESIAN_POINT('',(1.41899999999979,0.472999999999854,3.1));
#5001=CARTESIAN_POINT('Origin',(0.472999999999817,0.472999999999815,3.1));
#5002=CARTESIAN_POINT('',(2.36767196216383,0.472999999999892,2.87080111520185));
#5003=CARTESIAN_POINT('Origin',(-1.83061508724184E-14,0.472999999999796,
-9.73193776093083));
#5004=CARTESIAN_POINT('',(2.24662499999998,0.472999999999887,2.6611416266322));
#5005=CARTESIAN_POINT('Origin',(2.5,0.472999999999897,3.1));
#5006=CARTESIAN_POINT('',(2.36767196216383,-0.472999999999786,2.87080111520185));
#5007=CARTESIAN_POINT('Origin',(-3.68139204037345,0.,-7.60648507542867));
#5008=CARTESIAN_POINT('',(0.866098738193361,-0.65139580857508,0.270000000000001));
#5009=CARTESIAN_POINT('',(0.86609873819336,0.236499999999951,0.27));
#5010=CARTESIAN_POINT('',(1.41899999999987,-0.472999999999785,1.22765307701781));
#5011=CARTESIAN_POINT('Origin',(1.41899999999987,-1.41899999999979,1.22765307701781));
#5012=CARTESIAN_POINT('',(2.5,-0.472999999999786,3.1));
#5013=CARTESIAN_POINT('Origin',(2.5,-0.472999999999786,3.1));
#5014=CARTESIAN_POINT('',(1.41899999999987,-0.472999999999785,3.01252522110192));
#5015=CARTESIAN_POINT('Origin',(6.05980759185948E-16,-0.472999999999784,
-9.73193776093083));
#5016=CARTESIAN_POINT('',(1.41899999999987,-0.472999999999785,3.1));
#5017=CARTESIAN_POINT('Origin',(-1.41899999999978,-1.41899999999983,3.1));
#5018=CARTESIAN_POINT('',(-0.472999999999784,-1.41899999999984,3.01252522110192));
#5019=CARTESIAN_POINT('',(-1.41899999999983,-0.472999999999835,3.01252522110192));
#5020=CARTESIAN_POINT('Ctrl Pts',(-0.472999999999784,-1.41899999999984,
3.01252522110192));
#5021=CARTESIAN_POINT('Ctrl Pts',(-0.472999999999784,-1.41823784306299,
3.01261008153856));
#5022=CARTESIAN_POINT('Ctrl Pts',(-0.473000921064235,-1.41747599318126,
3.01269480438576));
#5023=CARTESIAN_POINT('Ctrl Pts',(-0.473287797471458,-1.29873656917597,
3.02588334070707));
#5024=CARTESIAN_POINT('Ctrl Pts',(-0.497030428020275,-1.17260477262755,
3.03726209636996));
#5025=CARTESIAN_POINT('Ctrl Pts',(-0.593452559529464,-0.940241249793266,
3.05235989856664));
#5026=CARTESIAN_POINT('Ctrl Pts',(-0.666140770092878,-0.834013199901788,
3.05607990145755));
#5027=CARTESIAN_POINT('Ctrl Pts',(-0.750076984997327,-0.750076984997344,
3.05607990145755));
#5028=CARTESIAN_POINT('Ctrl Pts',(-0.834013199901775,-0.6661407700929,3.05607990145755));
#5029=CARTESIAN_POINT('Ctrl Pts',(-0.940241249793256,-0.593452559529491,
3.05235989856665));
#5030=CARTESIAN_POINT('Ctrl Pts',(-1.17260477262755,-0.497030428020314,
3.03726209636996));
#5031=CARTESIAN_POINT('Ctrl Pts',(-1.29873656917596,-0.473287797471503,
3.02588334070706));
#5032=CARTESIAN_POINT('Ctrl Pts',(-1.41747599318109,-0.473000921064287,
3.01269480438577));
#5033=CARTESIAN_POINT('Ctrl Pts',(-1.41823784306282,-0.472999999999835,
3.01261008153858));
#5034=CARTESIAN_POINT('Ctrl Pts',(-1.41899999999983,-0.472999999999835,
3.01252522110192));
#5035=CARTESIAN_POINT('',(-0.472999999999784,-1.41899999999984,1.22765307701777));
#5036=CARTESIAN_POINT('',(-0.472999999999784,-1.41899999999984,3.1));
#5037=CARTESIAN_POINT('',(-0.651395808575061,-0.866098738193354,0.27));
#5038=CARTESIAN_POINT('Origin',(-1.41899999999978,-1.41899999999983,1.22765307701777));
#5039=CARTESIAN_POINT('',(-0.866098738193358,-0.651395808575073,0.27));
#5040=CARTESIAN_POINT('Origin',(-1.41899999999978,-1.41899999999983,0.27));
#5041=CARTESIAN_POINT('',(-1.41899999999983,-0.472999999999835,1.22765307701776));
#5042=CARTESIAN_POINT('Origin',(-1.41899999999978,-1.41899999999983,1.22765307701767));
#5043=CARTESIAN_POINT('',(-1.41899999999983,-0.472999999999835,3.1));
#5044=CARTESIAN_POINT('Origin',(-0.472999999999781,-0.472999999999784,3.1));
#5045=CARTESIAN_POINT('',(-2.36767196216382,-0.472999999999886,2.87080111520185));
#5046=CARTESIAN_POINT('Origin',(2.61729806275939E-14,-0.472999999999759,
-9.73193776093083));
#5047=CARTESIAN_POINT('',(-2.24662499999997,-0.472999999999879,2.66114162663219));
#5048=CARTESIAN_POINT('Origin',(1.41899999999987,-1.41899999999979,3.1));
#5049=CARTESIAN_POINT('',(0.472999999999865,-1.41899999999981,3.01252522110192));
#5050=CARTESIAN_POINT('Ctrl Pts',(1.41899999999987,-0.472999999999785,3.01252522110192));
#5051=CARTESIAN_POINT('Ctrl Pts',(1.41823784306302,-0.472999999999785,3.01261008153856));
#5052=CARTESIAN_POINT('Ctrl Pts',(1.41747599318129,-0.473000921064237,3.01269480438575));
#5053=CARTESIAN_POINT('Ctrl Pts',(1.29873656917601,-0.473287797471458,3.02588334070706));
#5054=CARTESIAN_POINT('Ctrl Pts',(1.17260477262759,-0.497030428020274,3.03726209636996));
#5055=CARTESIAN_POINT('Ctrl Pts',(0.940241249793305,-0.59345255952946,3.05235989856664));
#5056=CARTESIAN_POINT('Ctrl Pts',(0.834013199901827,-0.666140770092873,
3.05607990145755));
#5057=CARTESIAN_POINT('Ctrl Pts',(0.750076984997382,-0.75007698499732,3.05607990145755));
#5058=CARTESIAN_POINT('Ctrl Pts',(0.666140770092937,-0.834013199901768,
3.05607990145755));
#5059=CARTESIAN_POINT('Ctrl Pts',(0.593452559529527,-0.940241249793248,
3.05235989856665));
#5060=CARTESIAN_POINT('Ctrl Pts',(0.497030428020347,-1.17260477262754,3.03726209636996));
#5061=CARTESIAN_POINT('Ctrl Pts',(0.473287797471535,-1.29873656917595,3.02588334070706));
#5062=CARTESIAN_POINT('Ctrl Pts',(0.473000921064317,-1.41747599318107,3.01269480438577));
#5063=CARTESIAN_POINT('Ctrl Pts',(0.472999999999865,-1.4182378430628,3.01261008153858));
#5064=CARTESIAN_POINT('Ctrl Pts',(0.472999999999865,-1.41899999999981,3.01252522110192));
#5065=CARTESIAN_POINT('',(0.651395808575106,-0.866098738193356,0.27));
#5066=CARTESIAN_POINT('Origin',(1.41899999999987,-1.41899999999979,0.27));
#5067=CARTESIAN_POINT('',(0.472999999999865,-1.41899999999981,1.22765307701772));
#5068=CARTESIAN_POINT('Origin',(1.41899999999987,-1.41899999999979,1.22765307701768));
#5069=CARTESIAN_POINT('',(0.472999999999865,-1.41899999999981,3.1));
#5070=CARTESIAN_POINT('Origin',(0.472999999999839,-0.472999999999785,3.1));
#5071=CARTESIAN_POINT('',(0.472999999999892,-2.36767196216382,2.87080111520185));
#5072=CARTESIAN_POINT('Origin',(0.472999999999825,1.32935445800918E-14,
-9.73193776093083));
#5073=CARTESIAN_POINT('',(0.472999999999889,-2.24662499999997,2.66114162663219));
#5074=CARTESIAN_POINT('Origin',(-2.5,0.472999999999654,3.1));
#5075=CARTESIAN_POINT('',(-2.36767196216383,0.472999999999654,2.87080111520186));
#5076=CARTESIAN_POINT('Origin',(8.32667268468867E-16,0.472999999999654,
-9.73193776093083));
#5077=CARTESIAN_POINT('',(-2.5,0.472999999999654,3.1));
#5078=CARTESIAN_POINT('Origin',(-2.5,-0.472999999999893,3.1));
#5079=CARTESIAN_POINT('',(-2.37229341204248,-2.90522153369617E-16,2.87880570119631));
#5080=CARTESIAN_POINT('Origin',(3.68139204037345,0.,-7.60648507542867));
#5081=CARTESIAN_POINT('',(-0.866098738193358,-0.236499999999945,0.27));
#5082=CARTESIAN_POINT('Origin',(3.68139204037345,0.,-7.60648507542867));
#5083=CARTESIAN_POINT('Origin',(-0.472999999999788,-2.5,3.1));
#5084=CARTESIAN_POINT('',(-0.472999999999788,-2.36767196216382,2.87080111520185));
#5085=CARTESIAN_POINT('Origin',(-0.472999999999779,1.82968396778355E-15,
-9.73193776093083));
#5086=CARTESIAN_POINT('',(-0.472999999999788,-2.5,3.1));
#5087=CARTESIAN_POINT('Origin',(0.472999999999896,-2.5,3.1));
#5088=CARTESIAN_POINT('Origin',(6.23325686399709E-15,3.68139204037346,-7.60648507542867));
#5089=CARTESIAN_POINT('',(0.236499999999949,-0.866098738193356,0.27));
#5090=CARTESIAN_POINT('Origin',(1.11022302462516E-15,3.88578058618805E-15,
0.27));
#5091=CARTESIAN_POINT('Origin',(0.,0.,-0.2));
#5092=CARTESIAN_POINT('',(2.37846096908266,-2.91277461268399E-16,-3.46944695195361E-17));
#5093=CARTESIAN_POINT('Origin',(0.,0.,-3.46944695195361E-17));
#5094=CARTESIAN_POINT('',(2.17846096908266,-2.66784525285452E-16,-0.2));
#5095=CARTESIAN_POINT('Origin',(2.37846096908266,-2.91277461268399E-16,
-0.2));
#5096=CARTESIAN_POINT('Origin',(0.,0.,-0.2));
#5097=CARTESIAN_POINT('Origin',(-2.17846096908266,0.,-1.88141750998334E-17));
#5098=CARTESIAN_POINT('',(5.15,-6.30693101560887E-16,-2.77555756156289E-16));
#5099=CARTESIAN_POINT('Origin',(0.,0.,0.));
#5100=CARTESIAN_POINT('Origin',(0.,0.,-0.149999999999999));
#5101=CARTESIAN_POINT('',(2.17846096908266,-2.66784525285452E-16,-0.299999999999998));
#5102=CARTESIAN_POINT('Origin',(0.,0.,-0.299999999999998));
#5103=CARTESIAN_POINT('',(2.17846096908266,-2.66784525285452E-16,-0.149999999999999));
#5104=CARTESIAN_POINT('Origin',(0.,0.,-0.899999999999999));
#5105=CARTESIAN_POINT('',(2.4505,-3.00099698131059E-16,-1.31526348502534));
#5106=CARTESIAN_POINT('Origin',(0.,0.,-1.31526348502534));
#5107=CARTESIAN_POINT('',(2.33923048454133,-2.86473112536145E-16,-0.899999999999999));
#5108=CARTESIAN_POINT('Origin',(0.,0.,-7.75));
#5109=CARTESIAN_POINT('',(2.4505,3.00099698131059E-16,-14.));
#5110=CARTESIAN_POINT('Origin',(0.,0.,-14.));
#5111=CARTESIAN_POINT('',(2.4505,-3.00099698131059E-16,-7.75));
#5112=CARTESIAN_POINT('Origin',(0.,0.,-14.));
#5113=CARTESIAN_POINT('Origin',(8.32667268468867E-16,0.,-9.73193776093083));
#5114=CARTESIAN_POINT('',(-4.96627380657387,0.,2.1));
#5115=CARTESIAN_POINT('Origin',(8.32667268468867E-16,0.,-9.73193776093083));
#5116=CARTESIAN_POINT('',(4.96627380657386,-6.08193132091002E-16,2.1));
#5117=CARTESIAN_POINT('Origin',(0.,0.,2.1));
#5118=CARTESIAN_POINT('Origin',(0.,0.,2.1));
#5119=CARTESIAN_POINT('Origin',(0.,0.,1.05));
#5120=CARTESIAN_POINT('',(5.05813690328693,-6.19443116825945E-16,1.05));
#5121=CARTESIAN_POINT('',(0.,0.,0.));
#5122=CARTESIAN_POINT('Origin',(-1.41899999999985,1.41899999999965,3.1));
#5123=CARTESIAN_POINT('',(-1.41899999999985,0.472999999999654,3.01252522110193));
#5124=CARTESIAN_POINT('',(-0.472999999999848,1.41899999999969,3.01252522110194));
#5125=CARTESIAN_POINT('Ctrl Pts',(-1.41899999999985,0.472999999999654,3.01252522110193));
#5126=CARTESIAN_POINT('Ctrl Pts',(-1.418237843063,0.472999999999654,3.01261008153857));
#5127=CARTESIAN_POINT('Ctrl Pts',(-1.41747599318127,0.473000921064105,3.01269480438576));
#5128=CARTESIAN_POINT('Ctrl Pts',(-1.29873656917598,0.473287797471327,3.02588334070707));
#5129=CARTESIAN_POINT('Ctrl Pts',(-1.17260477262757,0.497030428020145,3.03726209636997));
#5130=CARTESIAN_POINT('Ctrl Pts',(-0.940241249793281,0.593452559529333,
3.05235989856665));
#5131=CARTESIAN_POINT('Ctrl Pts',(-0.834013199901804,0.666140770092746,
3.05607990145755));
#5132=CARTESIAN_POINT('Ctrl Pts',(-0.75007698499736,0.750076984997194,3.05607990145756));
#5133=CARTESIAN_POINT('Ctrl Pts',(-0.666140770092915,0.834013199901643,
3.05607990145756));
#5134=CARTESIAN_POINT('Ctrl Pts',(-0.593452559529506,0.940241249793123,
3.05235989856665));
#5135=CARTESIAN_POINT('Ctrl Pts',(-0.497030428020328,1.17260477262741,3.03726209636997));
#5136=CARTESIAN_POINT('Ctrl Pts',(-0.473287797471517,1.29873656917583,3.02588334070708));
#5137=CARTESIAN_POINT('Ctrl Pts',(-0.4730009210643,1.41747599318095,3.01269480438579));
#5138=CARTESIAN_POINT('Ctrl Pts',(-0.472999999999848,1.41823784306269,3.0126100815386));
#5139=CARTESIAN_POINT('Ctrl Pts',(-0.472999999999848,1.41899999999969,3.01252522110194));
#5140=CARTESIAN_POINT('',(-1.41899999999985,0.472999999999654,1.22765307701778));
#5141=CARTESIAN_POINT('',(-1.41899999999985,0.472999999999654,3.1));
#5142=CARTESIAN_POINT('',(-0.866098738193358,0.651395808574938,0.27));
#5143=CARTESIAN_POINT('Origin',(-1.41899999999985,1.41899999999965,1.22765307701778));
#5144=CARTESIAN_POINT('',(-0.651395808574991,0.86609873819336,0.27));
#5145=CARTESIAN_POINT('Origin',(-1.41899999999985,1.41899999999965,0.27));
#5146=CARTESIAN_POINT('',(-0.472999999999848,1.41899999999969,1.22765307701751));
#5147=CARTESIAN_POINT('Origin',(-1.41899999999985,1.41899999999965,1.22765307701745));
#5148=CARTESIAN_POINT('',(-0.472999999999848,1.41899999999969,3.1));
#5149=CARTESIAN_POINT('Origin',(-0.472999999999807,0.472999999999754,3.1));
#5150=CARTESIAN_POINT('',(-0.472999999999889,2.36767196216383,2.87080111520185));
#5151=CARTESIAN_POINT('Origin',(-0.472999999999787,-2.0353210154902E-14,
-9.73193776093083));
#5152=CARTESIAN_POINT('',(-0.472999999999884,2.24662499999997,2.66114162663218));
#5153=CARTESIAN_POINT('Origin',(-0.472999999999895,2.5,3.1));
#5154=CARTESIAN_POINT('',(0.472999999999787,2.36767196216383,2.87080111520185));
#5155=CARTESIAN_POINT('Origin',(1.16338464595253E-14,-3.68139204037345,
-7.60648507542867));
#5156=CARTESIAN_POINT('',(0.651395808575038,0.866098738193364,0.27));
#5157=CARTESIAN_POINT('',(-0.236499999999946,0.866098738193362,0.27));
#5158=CARTESIAN_POINT('',(0.472999999999754,1.41899999999989,1.22765307701784));
#5159=CARTESIAN_POINT('Origin',(1.41899999999975,1.41899999999985,1.22765307701778));
#5160=CARTESIAN_POINT('',(0.472999999999791,2.5,3.09999999999999));
#5161=CARTESIAN_POINT('Origin',(0.472999999999791,2.5,3.1));
#5162=CARTESIAN_POINT('',(0.472999999999754,1.41899999999989,3.01252522110192));
#5163=CARTESIAN_POINT('Origin',(0.472999999999705,-1.6370004348928E-14,
-9.73193776093083));
#5164=CARTESIAN_POINT('',(0.472999999999754,1.41899999999989,3.1));
#5165=CARTESIAN_POINT('Origin',(1.41899999999975,1.41899999999985,3.1));
#5166=CARTESIAN_POINT('',(1.41899999999979,0.472999999999854,3.01252522110193));
#5167=CARTESIAN_POINT('Ctrl Pts',(0.472999999999754,1.41899999999989,3.01252522110192));
#5168=CARTESIAN_POINT('Ctrl Pts',(0.472999999999754,1.41823784306304,3.01261008153856));
#5169=CARTESIAN_POINT('Ctrl Pts',(0.473000921064206,1.4174759931813,3.01269480438575));
#5170=CARTESIAN_POINT('Ctrl Pts',(0.473287797471426,1.29873656917601,3.02588334070706));
#5171=CARTESIAN_POINT('Ctrl Pts',(0.49703042802024,1.17260477262759,3.03726209636996));
#5172=CARTESIAN_POINT('Ctrl Pts',(0.593452559529424,0.940241249793303,3.05235989856665));
#5173=CARTESIAN_POINT('Ctrl Pts',(0.666140770092836,0.834013199901824,3.05607990145755));
#5174=CARTESIAN_POINT('Ctrl Pts',(0.750076984997282,0.750076984997378,3.05607990145755));
#5175=CARTESIAN_POINT('Ctrl Pts',(0.834013199901729,0.666140770092932,3.05607990145755));
#5176=CARTESIAN_POINT('Ctrl Pts',(0.940241249793208,0.593452559529521,3.05235989856665));
#5177=CARTESIAN_POINT('Ctrl Pts',(1.1726047726275,0.497030428020338,3.03726209636996));
#5178=CARTESIAN_POINT('Ctrl Pts',(1.29873656917591,0.473287797471525,3.02588334070707));
#5179=CARTESIAN_POINT('Ctrl Pts',(1.41747599318104,0.473000921064306,3.01269480438578));
#5180=CARTESIAN_POINT('Ctrl Pts',(1.41823784306278,0.472999999999854,3.01261008153858));
#5181=CARTESIAN_POINT('Ctrl Pts',(1.41899999999979,0.472999999999854,3.01252522110193));
#5182=CARTESIAN_POINT('',(0.866098738193361,0.651395808575069,0.27));
#5183=CARTESIAN_POINT('Origin',(1.41899999999975,1.41899999999985,0.27));
#5184=CARTESIAN_POINT('',(1.41899999999979,0.472999999999853,1.22765307701768));
#5185=CARTESIAN_POINT('Origin',(1.41899999999975,1.41899999999985,1.22765307701762));
#5186=CARTESIAN_POINT('',(1.41899999999979,0.472999999999854,3.1));
#5187=CARTESIAN_POINT('Origin',(0.472999999999817,0.472999999999815,3.1));
#5188=CARTESIAN_POINT('',(2.36767196216383,0.472999999999892,2.87080111520185));
#5189=CARTESIAN_POINT('Origin',(-1.83061508724184E-14,0.472999999999796,
-9.73193776093083));
#5190=CARTESIAN_POINT('',(2.24662499999998,0.472999999999887,2.6611416266322));
#5191=CARTESIAN_POINT('Origin',(2.5,0.472999999999897,3.1));
#5192=CARTESIAN_POINT('',(2.36767196216383,-0.472999999999786,2.87080111520185));
#5193=CARTESIAN_POINT('Origin',(-3.68139204037345,0.,-7.60648507542867));
#5194=CARTESIAN_POINT('',(0.866098738193361,-0.65139580857508,0.270000000000001));
#5195=CARTESIAN_POINT('',(0.86609873819336,0.236499999999951,0.27));
#5196=CARTESIAN_POINT('',(1.41899999999987,-0.472999999999785,1.22765307701781));
#5197=CARTESIAN_POINT('Origin',(1.41899999999987,-1.41899999999979,1.22765307701781));
#5198=CARTESIAN_POINT('',(2.5,-0.472999999999786,3.1));
#5199=CARTESIAN_POINT('Origin',(2.5,-0.472999999999786,3.1));
#5200=CARTESIAN_POINT('',(1.41899999999987,-0.472999999999785,3.01252522110192));
#5201=CARTESIAN_POINT('Origin',(6.05980759185948E-16,-0.472999999999784,
-9.73193776093083));
#5202=CARTESIAN_POINT('',(1.41899999999987,-0.472999999999785,3.1));
#5203=CARTESIAN_POINT('Origin',(-1.41899999999978,-1.41899999999983,3.1));
#5204=CARTESIAN_POINT('',(-0.472999999999784,-1.41899999999984,3.01252522110192));
#5205=CARTESIAN_POINT('',(-1.41899999999983,-0.472999999999835,3.01252522110192));
#5206=CARTESIAN_POINT('Ctrl Pts',(-0.472999999999784,-1.41899999999984,
3.01252522110192));
#5207=CARTESIAN_POINT('Ctrl Pts',(-0.472999999999784,-1.41823784306299,
3.01261008153856));
#5208=CARTESIAN_POINT('Ctrl Pts',(-0.473000921064235,-1.41747599318126,
3.01269480438576));
#5209=CARTESIAN_POINT('Ctrl Pts',(-0.473287797471458,-1.29873656917597,
3.02588334070707));
#5210=CARTESIAN_POINT('Ctrl Pts',(-0.497030428020275,-1.17260477262755,
3.03726209636996));
#5211=CARTESIAN_POINT('Ctrl Pts',(-0.593452559529464,-0.940241249793266,
3.05235989856664));
#5212=CARTESIAN_POINT('Ctrl Pts',(-0.666140770092878,-0.834013199901788,
3.05607990145755));
#5213=CARTESIAN_POINT('Ctrl Pts',(-0.750076984997327,-0.750076984997344,
3.05607990145755));
#5214=CARTESIAN_POINT('Ctrl Pts',(-0.834013199901775,-0.6661407700929,3.05607990145755));
#5215=CARTESIAN_POINT('Ctrl Pts',(-0.940241249793256,-0.593452559529491,
3.05235989856665));
#5216=CARTESIAN_POINT('Ctrl Pts',(-1.17260477262755,-0.497030428020314,
3.03726209636996));
#5217=CARTESIAN_POINT('Ctrl Pts',(-1.29873656917596,-0.473287797471503,
3.02588334070706));
#5218=CARTESIAN_POINT('Ctrl Pts',(-1.41747599318109,-0.473000921064287,
3.01269480438577));
#5219=CARTESIAN_POINT('Ctrl Pts',(-1.41823784306282,-0.472999999999835,
3.01261008153858));
#5220=CARTESIAN_POINT('Ctrl Pts',(-1.41899999999983,-0.472999999999835,
3.01252522110192));
#5221=CARTESIAN_POINT('',(-0.472999999999784,-1.41899999999984,1.22765307701777));
#5222=CARTESIAN_POINT('',(-0.472999999999784,-1.41899999999984,3.1));
#5223=CARTESIAN_POINT('',(-0.651395808575061,-0.866098738193354,0.27));
#5224=CARTESIAN_POINT('Origin',(-1.41899999999978,-1.41899999999983,1.22765307701777));
#5225=CARTESIAN_POINT('',(-0.866098738193358,-0.651395808575073,0.27));
#5226=CARTESIAN_POINT('Origin',(-1.41899999999978,-1.41899999999983,0.27));
#5227=CARTESIAN_POINT('',(-1.41899999999983,-0.472999999999835,1.22765307701776));
#5228=CARTESIAN_POINT('Origin',(-1.41899999999978,-1.41899999999983,1.22765307701767));
#5229=CARTESIAN_POINT('',(-1.41899999999983,-0.472999999999835,3.1));
#5230=CARTESIAN_POINT('Origin',(-0.472999999999781,-0.472999999999784,3.1));
#5231=CARTESIAN_POINT('',(-2.36767196216382,-0.472999999999886,2.87080111520185));
#5232=CARTESIAN_POINT('Origin',(2.61729806275939E-14,-0.472999999999759,
-9.73193776093083));
#5233=CARTESIAN_POINT('',(-2.24662499999997,-0.472999999999879,2.66114162663219));
#5234=CARTESIAN_POINT('Origin',(1.41899999999987,-1.41899999999979,3.1));
#5235=CARTESIAN_POINT('',(0.472999999999865,-1.41899999999981,3.01252522110192));
#5236=CARTESIAN_POINT('Ctrl Pts',(1.41899999999987,-0.472999999999785,3.01252522110192));
#5237=CARTESIAN_POINT('Ctrl Pts',(1.41823784306302,-0.472999999999785,3.01261008153856));
#5238=CARTESIAN_POINT('Ctrl Pts',(1.41747599318129,-0.473000921064237,3.01269480438575));
#5239=CARTESIAN_POINT('Ctrl Pts',(1.29873656917601,-0.473287797471458,3.02588334070706));
#5240=CARTESIAN_POINT('Ctrl Pts',(1.17260477262759,-0.497030428020274,3.03726209636996));
#5241=CARTESIAN_POINT('Ctrl Pts',(0.940241249793305,-0.59345255952946,3.05235989856664));
#5242=CARTESIAN_POINT('Ctrl Pts',(0.834013199901827,-0.666140770092873,
3.05607990145755));
#5243=CARTESIAN_POINT('Ctrl Pts',(0.750076984997382,-0.75007698499732,3.05607990145755));
#5244=CARTESIAN_POINT('Ctrl Pts',(0.666140770092937,-0.834013199901768,
3.05607990145755));
#5245=CARTESIAN_POINT('Ctrl Pts',(0.593452559529527,-0.940241249793248,
3.05235989856665));
#5246=CARTESIAN_POINT('Ctrl Pts',(0.497030428020347,-1.17260477262754,3.03726209636996));
#5247=CARTESIAN_POINT('Ctrl Pts',(0.473287797471535,-1.29873656917595,3.02588334070706));
#5248=CARTESIAN_POINT('Ctrl Pts',(0.473000921064317,-1.41747599318107,3.01269480438577));
#5249=CARTESIAN_POINT('Ctrl Pts',(0.472999999999865,-1.4182378430628,3.01261008153858));
#5250=CARTESIAN_POINT('Ctrl Pts',(0.472999999999865,-1.41899999999981,3.01252522110192));
#5251=CARTESIAN_POINT('',(0.651395808575106,-0.866098738193356,0.27));
#5252=CARTESIAN_POINT('Origin',(1.41899999999987,-1.41899999999979,0.27));
#5253=CARTESIAN_POINT('',(0.472999999999865,-1.41899999999981,1.22765307701772));
#5254=CARTESIAN_POINT('Origin',(1.41899999999987,-1.41899999999979,1.22765307701768));
#5255=CARTESIAN_POINT('',(0.472999999999865,-1.41899999999981,3.1));
#5256=CARTESIAN_POINT('Origin',(0.472999999999839,-0.472999999999785,3.1));
#5257=CARTESIAN_POINT('',(0.472999999999892,-2.36767196216382,2.87080111520185));
#5258=CARTESIAN_POINT('Origin',(0.472999999999825,1.32935445800918E-14,
-9.73193776093083));
#5259=CARTESIAN_POINT('',(0.472999999999889,-2.24662499999997,2.66114162663219));
#5260=CARTESIAN_POINT('Origin',(-2.5,0.472999999999654,3.1));
#5261=CARTESIAN_POINT('',(-2.36767196216383,0.472999999999654,2.87080111520186));
#5262=CARTESIAN_POINT('Origin',(8.32667268468867E-16,0.472999999999654,
-9.73193776093083));
#5263=CARTESIAN_POINT('',(-2.5,0.472999999999654,3.1));
#5264=CARTESIAN_POINT('Origin',(-2.5,-0.472999999999893,3.1));
#5265=CARTESIAN_POINT('',(-2.37229341204248,-2.90522153369617E-16,2.87880570119631));
#5266=CARTESIAN_POINT('Origin',(3.68139204037345,0.,-7.60648507542867));
#5267=CARTESIAN_POINT('',(-0.866098738193358,-0.236499999999945,0.27));
#5268=CARTESIAN_POINT('Origin',(3.68139204037345,0.,-7.60648507542867));
#5269=CARTESIAN_POINT('Origin',(-0.472999999999788,-2.5,3.1));
#5270=CARTESIAN_POINT('',(-0.472999999999788,-2.36767196216382,2.87080111520185));
#5271=CARTESIAN_POINT('Origin',(-0.472999999999779,1.82968396778355E-15,
-9.73193776093083));
#5272=CARTESIAN_POINT('',(-0.472999999999788,-2.5,3.1));
#5273=CARTESIAN_POINT('Origin',(0.472999999999896,-2.5,3.1));
#5274=CARTESIAN_POINT('Origin',(6.23325686399709E-15,3.68139204037346,-7.60648507542867));
#5275=CARTESIAN_POINT('',(0.236499999999949,-0.866098738193356,0.27));
#5276=CARTESIAN_POINT('Origin',(1.11022302462516E-15,3.88578058618805E-15,
0.27));
#5277=CARTESIAN_POINT('Origin',(0.,0.,-0.2));
#5278=CARTESIAN_POINT('',(2.37846096908266,-2.91277461268399E-16,-3.46944695195361E-17));
#5279=CARTESIAN_POINT('Origin',(0.,0.,-3.46944695195361E-17));
#5280=CARTESIAN_POINT('',(2.17846096908266,-2.66784525285452E-16,-0.2));
#5281=CARTESIAN_POINT('Origin',(2.37846096908266,-2.91277461268399E-16,
-0.2));
#5282=CARTESIAN_POINT('Origin',(0.,0.,-0.2));
#5283=CARTESIAN_POINT('Origin',(-2.17846096908266,0.,-1.88141750998334E-17));
#5284=CARTESIAN_POINT('',(5.15,-6.30693101560887E-16,-2.77555756156289E-16));
#5285=CARTESIAN_POINT('Origin',(0.,0.,0.));
#5286=CARTESIAN_POINT('Origin',(0.,0.,-0.149999999999999));
#5287=CARTESIAN_POINT('',(2.17846096908266,-2.66784525285452E-16,-0.299999999999998));
#5288=CARTESIAN_POINT('Origin',(0.,0.,-0.299999999999998));
#5289=CARTESIAN_POINT('',(2.17846096908266,-2.66784525285452E-16,-0.149999999999999));
#5290=CARTESIAN_POINT('Origin',(0.,0.,-0.899999999999999));
#5291=CARTESIAN_POINT('',(2.4505,-3.00099698131059E-16,-1.31526348502534));
#5292=CARTESIAN_POINT('Origin',(0.,0.,-1.31526348502534));
#5293=CARTESIAN_POINT('',(2.33923048454133,-2.86473112536145E-16,-0.899999999999999));
#5294=CARTESIAN_POINT('Origin',(0.,0.,-7.75));
#5295=CARTESIAN_POINT('',(2.4505,3.00099698131059E-16,-14.));
#5296=CARTESIAN_POINT('Origin',(0.,0.,-14.));
#5297=CARTESIAN_POINT('',(2.4505,-3.00099698131059E-16,-7.75));
#5298=CARTESIAN_POINT('Origin',(0.,0.,-14.));
#5299=CARTESIAN_POINT('Origin',(8.32667268468867E-16,0.,-9.73193776093083));
#5300=CARTESIAN_POINT('',(-4.96627380657387,0.,2.1));
#5301=CARTESIAN_POINT('Origin',(8.32667268468867E-16,0.,-9.73193776093083));
#5302=CARTESIAN_POINT('',(4.96627380657386,-6.08193132091002E-16,2.1));
#5303=CARTESIAN_POINT('Origin',(0.,0.,2.1));
#5304=CARTESIAN_POINT('Origin',(0.,0.,2.1));
#5305=CARTESIAN_POINT('Origin',(0.,0.,1.05));
#5306=CARTESIAN_POINT('',(5.05813690328693,-6.19443116825945E-16,1.05));
#5307=CARTESIAN_POINT('',(0.,0.,0.));
#5308=CARTESIAN_POINT('Origin',(-1.41899999999985,1.41899999999965,3.1));
#5309=CARTESIAN_POINT('',(-1.41899999999985,0.472999999999654,3.01252522110193));
#5310=CARTESIAN_POINT('',(-0.472999999999848,1.41899999999969,3.01252522110194));
#5311=CARTESIAN_POINT('Ctrl Pts',(-1.41899999999985,0.472999999999654,3.01252522110193));
#5312=CARTESIAN_POINT('Ctrl Pts',(-1.418237843063,0.472999999999654,3.01261008153857));
#5313=CARTESIAN_POINT('Ctrl Pts',(-1.41747599318127,0.473000921064105,3.01269480438576));
#5314=CARTESIAN_POINT('Ctrl Pts',(-1.29873656917598,0.473287797471327,3.02588334070707));
#5315=CARTESIAN_POINT('Ctrl Pts',(-1.17260477262757,0.497030428020145,3.03726209636997));
#5316=CARTESIAN_POINT('Ctrl Pts',(-0.940241249793281,0.593452559529333,
3.05235989856665));
#5317=CARTESIAN_POINT('Ctrl Pts',(-0.834013199901804,0.666140770092746,
3.05607990145755));
#5318=CARTESIAN_POINT('Ctrl Pts',(-0.75007698499736,0.750076984997194,3.05607990145756));
#5319=CARTESIAN_POINT('Ctrl Pts',(-0.666140770092915,0.834013199901643,
3.05607990145756));
#5320=CARTESIAN_POINT('Ctrl Pts',(-0.593452559529506,0.940241249793123,
3.05235989856665));
#5321=CARTESIAN_POINT('Ctrl Pts',(-0.497030428020328,1.17260477262741,3.03726209636997));
#5322=CARTESIAN_POINT('Ctrl Pts',(-0.473287797471517,1.29873656917583,3.02588334070708));
#5323=CARTESIAN_POINT('Ctrl Pts',(-0.4730009210643,1.41747599318095,3.01269480438579));
#5324=CARTESIAN_POINT('Ctrl Pts',(-0.472999999999848,1.41823784306269,3.0126100815386));
#5325=CARTESIAN_POINT('Ctrl Pts',(-0.472999999999848,1.41899999999969,3.01252522110194));
#5326=CARTESIAN_POINT('',(-1.41899999999985,0.472999999999654,1.22765307701778));
#5327=CARTESIAN_POINT('',(-1.41899999999985,0.472999999999654,3.1));
#5328=CARTESIAN_POINT('',(-0.866098738193358,0.651395808574938,0.27));
#5329=CARTESIAN_POINT('Origin',(-1.41899999999985,1.41899999999965,1.22765307701778));
#5330=CARTESIAN_POINT('',(-0.651395808574991,0.86609873819336,0.27));
#5331=CARTESIAN_POINT('Origin',(-1.41899999999985,1.41899999999965,0.27));
#5332=CARTESIAN_POINT('',(-0.472999999999848,1.41899999999969,1.22765307701751));
#5333=CARTESIAN_POINT('Origin',(-1.41899999999985,1.41899999999965,1.22765307701745));
#5334=CARTESIAN_POINT('',(-0.472999999999848,1.41899999999969,3.1));
#5335=CARTESIAN_POINT('Origin',(-0.472999999999807,0.472999999999754,3.1));
#5336=CARTESIAN_POINT('',(-0.472999999999889,2.36767196216383,2.87080111520185));
#5337=CARTESIAN_POINT('Origin',(-0.472999999999787,-2.0353210154902E-14,
-9.73193776093083));
#5338=CARTESIAN_POINT('',(-0.472999999999884,2.24662499999997,2.66114162663218));
#5339=CARTESIAN_POINT('Origin',(-0.472999999999895,2.5,3.1));
#5340=CARTESIAN_POINT('',(0.472999999999787,2.36767196216383,2.87080111520185));
#5341=CARTESIAN_POINT('Origin',(1.16338464595253E-14,-3.68139204037345,
-7.60648507542867));
#5342=CARTESIAN_POINT('',(0.651395808575038,0.866098738193364,0.27));
#5343=CARTESIAN_POINT('',(-0.236499999999946,0.866098738193362,0.27));
#5344=CARTESIAN_POINT('',(0.472999999999754,1.41899999999989,1.22765307701784));
#5345=CARTESIAN_POINT('Origin',(1.41899999999975,1.41899999999985,1.22765307701778));
#5346=CARTESIAN_POINT('',(0.472999999999791,2.5,3.09999999999999));
#5347=CARTESIAN_POINT('Origin',(0.472999999999791,2.5,3.1));
#5348=CARTESIAN_POINT('',(0.472999999999754,1.41899999999989,3.01252522110192));
#5349=CARTESIAN_POINT('Origin',(0.472999999999705,-1.6370004348928E-14,
-9.73193776093083));
#5350=CARTESIAN_POINT('',(0.472999999999754,1.41899999999989,3.1));
#5351=CARTESIAN_POINT('Origin',(1.41899999999975,1.41899999999985,3.1));
#5352=CARTESIAN_POINT('',(1.41899999999979,0.472999999999854,3.01252522110193));
#5353=CARTESIAN_POINT('Ctrl Pts',(0.472999999999754,1.41899999999989,3.01252522110192));
#5354=CARTESIAN_POINT('Ctrl Pts',(0.472999999999754,1.41823784306304,3.01261008153856));
#5355=CARTESIAN_POINT('Ctrl Pts',(0.473000921064206,1.4174759931813,3.01269480438575));
#5356=CARTESIAN_POINT('Ctrl Pts',(0.473287797471426,1.29873656917601,3.02588334070706));
#5357=CARTESIAN_POINT('Ctrl Pts',(0.49703042802024,1.17260477262759,3.03726209636996));
#5358=CARTESIAN_POINT('Ctrl Pts',(0.593452559529424,0.940241249793303,3.05235989856665));
#5359=CARTESIAN_POINT('Ctrl Pts',(0.666140770092836,0.834013199901824,3.05607990145755));
#5360=CARTESIAN_POINT('Ctrl Pts',(0.750076984997282,0.750076984997378,3.05607990145755));
#5361=CARTESIAN_POINT('Ctrl Pts',(0.834013199901729,0.666140770092932,3.05607990145755));
#5362=CARTESIAN_POINT('Ctrl Pts',(0.940241249793208,0.593452559529521,3.05235989856665));
#5363=CARTESIAN_POINT('Ctrl Pts',(1.1726047726275,0.497030428020338,3.03726209636996));
#5364=CARTESIAN_POINT('Ctrl Pts',(1.29873656917591,0.473287797471525,3.02588334070707));
#5365=CARTESIAN_POINT('Ctrl Pts',(1.41747599318104,0.473000921064306,3.01269480438578));
#5366=CARTESIAN_POINT('Ctrl Pts',(1.41823784306278,0.472999999999854,3.01261008153858));
#5367=CARTESIAN_POINT('Ctrl Pts',(1.41899999999979,0.472999999999854,3.01252522110193));
#5368=CARTESIAN_POINT('',(0.866098738193361,0.651395808575069,0.27));
#5369=CARTESIAN_POINT('Origin',(1.41899999999975,1.41899999999985,0.27));
#5370=CARTESIAN_POINT('',(1.41899999999979,0.472999999999853,1.22765307701768));
#5371=CARTESIAN_POINT('Origin',(1.41899999999975,1.41899999999985,1.22765307701762));
#5372=CARTESIAN_POINT('',(1.41899999999979,0.472999999999854,3.1));
#5373=CARTESIAN_POINT('Origin',(0.472999999999817,0.472999999999815,3.1));
#5374=CARTESIAN_POINT('',(2.36767196216383,0.472999999999892,2.87080111520185));
#5375=CARTESIAN_POINT('Origin',(-1.83061508724184E-14,0.472999999999796,
-9.73193776093083));
#5376=CARTESIAN_POINT('',(2.24662499999998,0.472999999999887,2.6611416266322));
#5377=CARTESIAN_POINT('Origin',(2.5,0.472999999999897,3.1));
#5378=CARTESIAN_POINT('',(2.36767196216383,-0.472999999999786,2.87080111520185));
#5379=CARTESIAN_POINT('Origin',(-3.68139204037345,0.,-7.60648507542867));
#5380=CARTESIAN_POINT('',(0.866098738193361,-0.65139580857508,0.270000000000001));
#5381=CARTESIAN_POINT('',(0.86609873819336,0.236499999999951,0.27));
#5382=CARTESIAN_POINT('',(1.41899999999987,-0.472999999999785,1.22765307701781));
#5383=CARTESIAN_POINT('Origin',(1.41899999999987,-1.41899999999979,1.22765307701781));
#5384=CARTESIAN_POINT('',(2.5,-0.472999999999786,3.1));
#5385=CARTESIAN_POINT('Origin',(2.5,-0.472999999999786,3.1));
#5386=CARTESIAN_POINT('',(1.41899999999987,-0.472999999999785,3.01252522110192));
#5387=CARTESIAN_POINT('Origin',(6.05980759185948E-16,-0.472999999999784,
-9.73193776093083));
#5388=CARTESIAN_POINT('',(1.41899999999987,-0.472999999999785,3.1));
#5389=CARTESIAN_POINT('Origin',(-1.41899999999978,-1.41899999999983,3.1));
#5390=CARTESIAN_POINT('',(-0.472999999999784,-1.41899999999984,3.01252522110192));
#5391=CARTESIAN_POINT('',(-1.41899999999983,-0.472999999999835,3.01252522110192));
#5392=CARTESIAN_POINT('Ctrl Pts',(-0.472999999999784,-1.41899999999984,
3.01252522110192));
#5393=CARTESIAN_POINT('Ctrl Pts',(-0.472999999999784,-1.41823784306299,
3.01261008153856));
#5394=CARTESIAN_POINT('Ctrl Pts',(-0.473000921064235,-1.41747599318126,
3.01269480438576));
#5395=CARTESIAN_POINT('Ctrl Pts',(-0.473287797471458,-1.29873656917597,
3.02588334070707));
#5396=CARTESIAN_POINT('Ctrl Pts',(-0.497030428020275,-1.17260477262755,
3.03726209636996));
#5397=CARTESIAN_POINT('Ctrl Pts',(-0.593452559529464,-0.940241249793266,
3.05235989856664));
#5398=CARTESIAN_POINT('Ctrl Pts',(-0.666140770092878,-0.834013199901788,
3.05607990145755));
#5399=CARTESIAN_POINT('Ctrl Pts',(-0.750076984997327,-0.750076984997344,
3.05607990145755));
#5400=CARTESIAN_POINT('Ctrl Pts',(-0.834013199901775,-0.6661407700929,3.05607990145755));
#5401=CARTESIAN_POINT('Ctrl Pts',(-0.940241249793256,-0.593452559529491,
3.05235989856665));
#5402=CARTESIAN_POINT('Ctrl Pts',(-1.17260477262755,-0.497030428020314,
3.03726209636996));
#5403=CARTESIAN_POINT('Ctrl Pts',(-1.29873656917596,-0.473287797471503,
3.02588334070706));
#5404=CARTESIAN_POINT('Ctrl Pts',(-1.41747599318109,-0.473000921064287,
3.01269480438577));
#5405=CARTESIAN_POINT('Ctrl Pts',(-1.41823784306282,-0.472999999999835,
3.01261008153858));
#5406=CARTESIAN_POINT('Ctrl Pts',(-1.41899999999983,-0.472999999999835,
3.01252522110192));
#5407=CARTESIAN_POINT('',(-0.472999999999784,-1.41899999999984,1.22765307701777));
#5408=CARTESIAN_POINT('',(-0.472999999999784,-1.41899999999984,3.1));
#5409=CARTESIAN_POINT('',(-0.651395808575061,-0.866098738193354,0.27));
#5410=CARTESIAN_POINT('Origin',(-1.41899999999978,-1.41899999999983,1.22765307701777));
#5411=CARTESIAN_POINT('',(-0.866098738193358,-0.651395808575073,0.27));
#5412=CARTESIAN_POINT('Origin',(-1.41899999999978,-1.41899999999983,0.27));
#5413=CARTESIAN_POINT('',(-1.41899999999983,-0.472999999999835,1.22765307701776));
#5414=CARTESIAN_POINT('Origin',(-1.41899999999978,-1.41899999999983,1.22765307701767));
#5415=CARTESIAN_POINT('',(-1.41899999999983,-0.472999999999835,3.1));
#5416=CARTESIAN_POINT('Origin',(-0.472999999999781,-0.472999999999784,3.1));
#5417=CARTESIAN_POINT('',(-2.36767196216382,-0.472999999999886,2.87080111520185));
#5418=CARTESIAN_POINT('Origin',(2.61729806275939E-14,-0.472999999999759,
-9.73193776093083));
#5419=CARTESIAN_POINT('',(-2.24662499999997,-0.472999999999879,2.66114162663219));
#5420=CARTESIAN_POINT('Origin',(1.41899999999987,-1.41899999999979,3.1));
#5421=CARTESIAN_POINT('',(0.472999999999865,-1.41899999999981,3.01252522110192));
#5422=CARTESIAN_POINT('Ctrl Pts',(1.41899999999987,-0.472999999999785,3.01252522110192));
#5423=CARTESIAN_POINT('Ctrl Pts',(1.41823784306302,-0.472999999999785,3.01261008153856));
#5424=CARTESIAN_POINT('Ctrl Pts',(1.41747599318129,-0.473000921064237,3.01269480438575));
#5425=CARTESIAN_POINT('Ctrl Pts',(1.29873656917601,-0.473287797471458,3.02588334070706));
#5426=CARTESIAN_POINT('Ctrl Pts',(1.17260477262759,-0.497030428020274,3.03726209636996));
#5427=CARTESIAN_POINT('Ctrl Pts',(0.940241249793305,-0.59345255952946,3.05235989856664));
#5428=CARTESIAN_POINT('Ctrl Pts',(0.834013199901827,-0.666140770092873,
3.05607990145755));
#5429=CARTESIAN_POINT('Ctrl Pts',(0.750076984997382,-0.75007698499732,3.05607990145755));
#5430=CARTESIAN_POINT('Ctrl Pts',(0.666140770092937,-0.834013199901768,
3.05607990145755));
#5431=CARTESIAN_POINT('Ctrl Pts',(0.593452559529527,-0.940241249793248,
3.05235989856665));
#5432=CARTESIAN_POINT('Ctrl Pts',(0.497030428020347,-1.17260477262754,3.03726209636996));
#5433=CARTESIAN_POINT('Ctrl Pts',(0.473287797471535,-1.29873656917595,3.02588334070706));
#5434=CARTESIAN_POINT('Ctrl Pts',(0.473000921064317,-1.41747599318107,3.01269480438577));
#5435=CARTESIAN_POINT('Ctrl Pts',(0.472999999999865,-1.4182378430628,3.01261008153858));
#5436=CARTESIAN_POINT('Ctrl Pts',(0.472999999999865,-1.41899999999981,3.01252522110192));
#5437=CARTESIAN_POINT('',(0.651395808575106,-0.866098738193356,0.27));
#5438=CARTESIAN_POINT('Origin',(1.41899999999987,-1.41899999999979,0.27));
#5439=CARTESIAN_POINT('',(0.472999999999865,-1.41899999999981,1.22765307701772));
#5440=CARTESIAN_POINT('Origin',(1.41899999999987,-1.41899999999979,1.22765307701768));
#5441=CARTESIAN_POINT('',(0.472999999999865,-1.41899999999981,3.1));
#5442=CARTESIAN_POINT('Origin',(0.472999999999839,-0.472999999999785,3.1));
#5443=CARTESIAN_POINT('',(0.472999999999892,-2.36767196216382,2.87080111520185));
#5444=CARTESIAN_POINT('Origin',(0.472999999999825,1.32935445800918E-14,
-9.73193776093083));
#5445=CARTESIAN_POINT('',(0.472999999999889,-2.24662499999997,2.66114162663219));
#5446=CARTESIAN_POINT('Origin',(-2.5,0.472999999999654,3.1));
#5447=CARTESIAN_POINT('',(-2.36767196216383,0.472999999999654,2.87080111520186));
#5448=CARTESIAN_POINT('Origin',(8.32667268468867E-16,0.472999999999654,
-9.73193776093083));
#5449=CARTESIAN_POINT('',(-2.5,0.472999999999654,3.1));
#5450=CARTESIAN_POINT('Origin',(-2.5,-0.472999999999893,3.1));
#5451=CARTESIAN_POINT('',(-2.37229341204248,-2.90522153369617E-16,2.87880570119631));
#5452=CARTESIAN_POINT('Origin',(3.68139204037345,0.,-7.60648507542867));
#5453=CARTESIAN_POINT('',(-0.866098738193358,-0.236499999999945,0.27));
#5454=CARTESIAN_POINT('Origin',(3.68139204037345,0.,-7.60648507542867));
#5455=CARTESIAN_POINT('Origin',(-0.472999999999788,-2.5,3.1));
#5456=CARTESIAN_POINT('',(-0.472999999999788,-2.36767196216382,2.87080111520185));
#5457=CARTESIAN_POINT('Origin',(-0.472999999999779,1.82968396778355E-15,
-9.73193776093083));
#5458=CARTESIAN_POINT('',(-0.472999999999788,-2.5,3.1));
#5459=CARTESIAN_POINT('Origin',(0.472999999999896,-2.5,3.1));
#5460=CARTESIAN_POINT('Origin',(6.23325686399709E-15,3.68139204037346,-7.60648507542867));
#5461=CARTESIAN_POINT('',(0.236499999999949,-0.866098738193356,0.27));
#5462=CARTESIAN_POINT('Origin',(1.11022302462516E-15,3.88578058618805E-15,
0.27));
#5463=CARTESIAN_POINT('Origin',(0.,0.,-0.2));
#5464=CARTESIAN_POINT('',(2.37846096908266,-2.91277461268399E-16,-3.46944695195361E-17));
#5465=CARTESIAN_POINT('Origin',(0.,0.,-3.46944695195361E-17));
#5466=CARTESIAN_POINT('',(2.17846096908266,-2.66784525285452E-16,-0.2));
#5467=CARTESIAN_POINT('Origin',(2.37846096908266,-2.91277461268399E-16,
-0.2));
#5468=CARTESIAN_POINT('Origin',(0.,0.,-0.2));
#5469=CARTESIAN_POINT('Origin',(-2.17846096908266,0.,-1.88141750998334E-17));
#5470=CARTESIAN_POINT('',(5.15,-6.30693101560887E-16,-2.77555756156289E-16));
#5471=CARTESIAN_POINT('Origin',(0.,0.,0.));
#5472=CARTESIAN_POINT('Origin',(0.,0.,-0.149999999999999));
#5473=CARTESIAN_POINT('',(2.17846096908266,-2.66784525285452E-16,-0.299999999999998));
#5474=CARTESIAN_POINT('Origin',(0.,0.,-0.299999999999998));
#5475=CARTESIAN_POINT('',(2.17846096908266,-2.66784525285452E-16,-0.149999999999999));
#5476=CARTESIAN_POINT('Origin',(0.,0.,-0.899999999999999));
#5477=CARTESIAN_POINT('',(2.4505,-3.00099698131059E-16,-1.31526348502534));
#5478=CARTESIAN_POINT('Origin',(0.,0.,-1.31526348502534));
#5479=CARTESIAN_POINT('',(2.33923048454133,-2.86473112536145E-16,-0.899999999999999));
#5480=CARTESIAN_POINT('Origin',(0.,0.,-7.75));
#5481=CARTESIAN_POINT('',(2.4505,3.00099698131059E-16,-14.));
#5482=CARTESIAN_POINT('Origin',(0.,0.,-14.));
#5483=CARTESIAN_POINT('',(2.4505,-3.00099698131059E-16,-7.75));
#5484=CARTESIAN_POINT('Origin',(0.,0.,-14.));
#5485=CARTESIAN_POINT('Origin',(8.32667268468867E-16,0.,-9.73193776093083));
#5486=CARTESIAN_POINT('',(-4.96627380657387,0.,2.1));
#5487=CARTESIAN_POINT('Origin',(8.32667268468867E-16,0.,-9.73193776093083));
#5488=CARTESIAN_POINT('',(4.96627380657386,-6.08193132091002E-16,2.1));
#5489=CARTESIAN_POINT('Origin',(0.,0.,2.1));
#5490=CARTESIAN_POINT('Origin',(0.,0.,2.1));
#5491=CARTESIAN_POINT('Origin',(0.,0.,1.05));
#5492=CARTESIAN_POINT('',(5.05813690328693,-6.19443116825945E-16,1.05));
#5493=CARTESIAN_POINT('',(0.,0.,0.));
#5494=CARTESIAN_POINT('Origin',(-1.41899999999985,1.41899999999965,3.1));
#5495=CARTESIAN_POINT('',(-1.41899999999985,0.472999999999654,3.01252522110193));
#5496=CARTESIAN_POINT('',(-0.472999999999848,1.41899999999969,3.01252522110194));
#5497=CARTESIAN_POINT('Ctrl Pts',(-1.41899999999985,0.472999999999654,3.01252522110193));
#5498=CARTESIAN_POINT('Ctrl Pts',(-1.418237843063,0.472999999999654,3.01261008153857));
#5499=CARTESIAN_POINT('Ctrl Pts',(-1.41747599318127,0.473000921064105,3.01269480438576));
#5500=CARTESIAN_POINT('Ctrl Pts',(-1.29873656917598,0.473287797471327,3.02588334070707));
#5501=CARTESIAN_POINT('Ctrl Pts',(-1.17260477262757,0.497030428020145,3.03726209636997));
#5502=CARTESIAN_POINT('Ctrl Pts',(-0.940241249793281,0.593452559529333,
3.05235989856665));
#5503=CARTESIAN_POINT('Ctrl Pts',(-0.834013199901804,0.666140770092746,
3.05607990145755));
#5504=CARTESIAN_POINT('Ctrl Pts',(-0.75007698499736,0.750076984997194,3.05607990145756));
#5505=CARTESIAN_POINT('Ctrl Pts',(-0.666140770092915,0.834013199901643,
3.05607990145756));
#5506=CARTESIAN_POINT('Ctrl Pts',(-0.593452559529506,0.940241249793123,
3.05235989856665));
#5507=CARTESIAN_POINT('Ctrl Pts',(-0.497030428020328,1.17260477262741,3.03726209636997));
#5508=CARTESIAN_POINT('Ctrl Pts',(-0.473287797471517,1.29873656917583,3.02588334070708));
#5509=CARTESIAN_POINT('Ctrl Pts',(-0.4730009210643,1.41747599318095,3.01269480438579));
#5510=CARTESIAN_POINT('Ctrl Pts',(-0.472999999999848,1.41823784306269,3.0126100815386));
#5511=CARTESIAN_POINT('Ctrl Pts',(-0.472999999999848,1.41899999999969,3.01252522110194));
#5512=CARTESIAN_POINT('',(-1.41899999999985,0.472999999999654,1.22765307701778));
#5513=CARTESIAN_POINT('',(-1.41899999999985,0.472999999999654,3.1));
#5514=CARTESIAN_POINT('',(-0.866098738193358,0.651395808574938,0.27));
#5515=CARTESIAN_POINT('Origin',(-1.41899999999985,1.41899999999965,1.22765307701778));
#5516=CARTESIAN_POINT('',(-0.651395808574991,0.86609873819336,0.27));
#5517=CARTESIAN_POINT('Origin',(-1.41899999999985,1.41899999999965,0.27));
#5518=CARTESIAN_POINT('',(-0.472999999999848,1.41899999999969,1.22765307701751));
#5519=CARTESIAN_POINT('Origin',(-1.41899999999985,1.41899999999965,1.22765307701745));
#5520=CARTESIAN_POINT('',(-0.472999999999848,1.41899999999969,3.1));
#5521=CARTESIAN_POINT('Origin',(-0.472999999999807,0.472999999999754,3.1));
#5522=CARTESIAN_POINT('',(-0.472999999999889,2.36767196216383,2.87080111520185));
#5523=CARTESIAN_POINT('Origin',(-0.472999999999787,-2.0353210154902E-14,
-9.73193776093083));
#5524=CARTESIAN_POINT('',(-0.472999999999884,2.24662499999997,2.66114162663218));
#5525=CARTESIAN_POINT('Origin',(-0.472999999999895,2.5,3.1));
#5526=CARTESIAN_POINT('',(0.472999999999787,2.36767196216383,2.87080111520185));
#5527=CARTESIAN_POINT('Origin',(1.16338464595253E-14,-3.68139204037345,
-7.60648507542867));
#5528=CARTESIAN_POINT('',(0.651395808575038,0.866098738193364,0.27));
#5529=CARTESIAN_POINT('',(-0.236499999999946,0.866098738193362,0.27));
#5530=CARTESIAN_POINT('',(0.472999999999754,1.41899999999989,1.22765307701784));
#5531=CARTESIAN_POINT('Origin',(1.41899999999975,1.41899999999985,1.22765307701778));
#5532=CARTESIAN_POINT('',(0.472999999999791,2.5,3.09999999999999));
#5533=CARTESIAN_POINT('Origin',(0.472999999999791,2.5,3.1));
#5534=CARTESIAN_POINT('',(0.472999999999754,1.41899999999989,3.01252522110192));
#5535=CARTESIAN_POINT('Origin',(0.472999999999705,-1.6370004348928E-14,
-9.73193776093083));
#5536=CARTESIAN_POINT('',(0.472999999999754,1.41899999999989,3.1));
#5537=CARTESIAN_POINT('Origin',(1.41899999999975,1.41899999999985,3.1));
#5538=CARTESIAN_POINT('',(1.41899999999979,0.472999999999854,3.01252522110193));
#5539=CARTESIAN_POINT('Ctrl Pts',(0.472999999999754,1.41899999999989,3.01252522110192));
#5540=CARTESIAN_POINT('Ctrl Pts',(0.472999999999754,1.41823784306304,3.01261008153856));
#5541=CARTESIAN_POINT('Ctrl Pts',(0.473000921064206,1.4174759931813,3.01269480438575));
#5542=CARTESIAN_POINT('Ctrl Pts',(0.473287797471426,1.29873656917601,3.02588334070706));
#5543=CARTESIAN_POINT('Ctrl Pts',(0.49703042802024,1.17260477262759,3.03726209636996));
#5544=CARTESIAN_POINT('Ctrl Pts',(0.593452559529424,0.940241249793303,3.05235989856665));
#5545=CARTESIAN_POINT('Ctrl Pts',(0.666140770092836,0.834013199901824,3.05607990145755));
#5546=CARTESIAN_POINT('Ctrl Pts',(0.750076984997282,0.750076984997378,3.05607990145755));
#5547=CARTESIAN_POINT('Ctrl Pts',(0.834013199901729,0.666140770092932,3.05607990145755));
#5548=CARTESIAN_POINT('Ctrl Pts',(0.940241249793208,0.593452559529521,3.05235989856665));
#5549=CARTESIAN_POINT('Ctrl Pts',(1.1726047726275,0.497030428020338,3.03726209636996));
#5550=CARTESIAN_POINT('Ctrl Pts',(1.29873656917591,0.473287797471525,3.02588334070707));
#5551=CARTESIAN_POINT('Ctrl Pts',(1.41747599318104,0.473000921064306,3.01269480438578));
#5552=CARTESIAN_POINT('Ctrl Pts',(1.41823784306278,0.472999999999854,3.01261008153858));
#5553=CARTESIAN_POINT('Ctrl Pts',(1.41899999999979,0.472999999999854,3.01252522110193));
#5554=CARTESIAN_POINT('',(0.866098738193361,0.651395808575069,0.27));
#5555=CARTESIAN_POINT('Origin',(1.41899999999975,1.41899999999985,0.27));
#5556=CARTESIAN_POINT('',(1.41899999999979,0.472999999999853,1.22765307701768));
#5557=CARTESIAN_POINT('Origin',(1.41899999999975,1.41899999999985,1.22765307701762));
#5558=CARTESIAN_POINT('',(1.41899999999979,0.472999999999854,3.1));
#5559=CARTESIAN_POINT('Origin',(0.472999999999817,0.472999999999815,3.1));
#5560=CARTESIAN_POINT('',(2.36767196216383,0.472999999999892,2.87080111520185));
#5561=CARTESIAN_POINT('Origin',(-1.83061508724184E-14,0.472999999999796,
-9.73193776093083));
#5562=CARTESIAN_POINT('',(2.24662499999998,0.472999999999887,2.6611416266322));
#5563=CARTESIAN_POINT('Origin',(2.5,0.472999999999897,3.1));
#5564=CARTESIAN_POINT('',(2.36767196216383,-0.472999999999786,2.87080111520185));
#5565=CARTESIAN_POINT('Origin',(-3.68139204037345,0.,-7.60648507542867));
#5566=CARTESIAN_POINT('',(0.866098738193361,-0.65139580857508,0.270000000000001));
#5567=CARTESIAN_POINT('',(0.86609873819336,0.236499999999951,0.27));
#5568=CARTESIAN_POINT('',(1.41899999999987,-0.472999999999785,1.22765307701781));
#5569=CARTESIAN_POINT('Origin',(1.41899999999987,-1.41899999999979,1.22765307701781));
#5570=CARTESIAN_POINT('',(2.5,-0.472999999999786,3.1));
#5571=CARTESIAN_POINT('Origin',(2.5,-0.472999999999786,3.1));
#5572=CARTESIAN_POINT('',(1.41899999999987,-0.472999999999785,3.01252522110192));
#5573=CARTESIAN_POINT('Origin',(6.05980759185948E-16,-0.472999999999784,
-9.73193776093083));
#5574=CARTESIAN_POINT('',(1.41899999999987,-0.472999999999785,3.1));
#5575=CARTESIAN_POINT('Origin',(-1.41899999999978,-1.41899999999983,3.1));
#5576=CARTESIAN_POINT('',(-0.472999999999784,-1.41899999999984,3.01252522110192));
#5577=CARTESIAN_POINT('',(-1.41899999999983,-0.472999999999835,3.01252522110192));
#5578=CARTESIAN_POINT('Ctrl Pts',(-0.472999999999784,-1.41899999999984,
3.01252522110192));
#5579=CARTESIAN_POINT('Ctrl Pts',(-0.472999999999784,-1.41823784306299,
3.01261008153856));
#5580=CARTESIAN_POINT('Ctrl Pts',(-0.473000921064235,-1.41747599318126,
3.01269480438576));
#5581=CARTESIAN_POINT('Ctrl Pts',(-0.473287797471458,-1.29873656917597,
3.02588334070707));
#5582=CARTESIAN_POINT('Ctrl Pts',(-0.497030428020275,-1.17260477262755,
3.03726209636996));
#5583=CARTESIAN_POINT('Ctrl Pts',(-0.593452559529464,-0.940241249793266,
3.05235989856664));
#5584=CARTESIAN_POINT('Ctrl Pts',(-0.666140770092878,-0.834013199901788,
3.05607990145755));
#5585=CARTESIAN_POINT('Ctrl Pts',(-0.750076984997327,-0.750076984997344,
3.05607990145755));
#5586=CARTESIAN_POINT('Ctrl Pts',(-0.834013199901775,-0.6661407700929,3.05607990145755));
#5587=CARTESIAN_POINT('Ctrl Pts',(-0.940241249793256,-0.593452559529491,
3.05235989856665));
#5588=CARTESIAN_POINT('Ctrl Pts',(-1.17260477262755,-0.497030428020314,
3.03726209636996));
#5589=CARTESIAN_POINT('Ctrl Pts',(-1.29873656917596,-0.473287797471503,
3.02588334070706));
#5590=CARTESIAN_POINT('Ctrl Pts',(-1.41747599318109,-0.473000921064287,
3.01269480438577));
#5591=CARTESIAN_POINT('Ctrl Pts',(-1.41823784306282,-0.472999999999835,
3.01261008153858));
#5592=CARTESIAN_POINT('Ctrl Pts',(-1.41899999999983,-0.472999999999835,
3.01252522110192));
#5593=CARTESIAN_POINT('',(-0.472999999999784,-1.41899999999984,1.22765307701777));
#5594=CARTESIAN_POINT('',(-0.472999999999784,-1.41899999999984,3.1));
#5595=CARTESIAN_POINT('',(-0.651395808575061,-0.866098738193354,0.27));
#5596=CARTESIAN_POINT('Origin',(-1.41899999999978,-1.41899999999983,1.22765307701777));
#5597=CARTESIAN_POINT('',(-0.866098738193358,-0.651395808575073,0.27));
#5598=CARTESIAN_POINT('Origin',(-1.41899999999978,-1.41899999999983,0.27));
#5599=CARTESIAN_POINT('',(-1.41899999999983,-0.472999999999835,1.22765307701776));
#5600=CARTESIAN_POINT('Origin',(-1.41899999999978,-1.41899999999983,1.22765307701767));
#5601=CARTESIAN_POINT('',(-1.41899999999983,-0.472999999999835,3.1));
#5602=CARTESIAN_POINT('Origin',(-0.472999999999781,-0.472999999999784,3.1));
#5603=CARTESIAN_POINT('',(-2.36767196216382,-0.472999999999886,2.87080111520185));
#5604=CARTESIAN_POINT('Origin',(2.61729806275939E-14,-0.472999999999759,
-9.73193776093083));
#5605=CARTESIAN_POINT('',(-2.24662499999997,-0.472999999999879,2.66114162663219));
#5606=CARTESIAN_POINT('Origin',(1.41899999999987,-1.41899999999979,3.1));
#5607=CARTESIAN_POINT('',(0.472999999999865,-1.41899999999981,3.01252522110192));
#5608=CARTESIAN_POINT('Ctrl Pts',(1.41899999999987,-0.472999999999785,3.01252522110192));
#5609=CARTESIAN_POINT('Ctrl Pts',(1.41823784306302,-0.472999999999785,3.01261008153856));
#5610=CARTESIAN_POINT('Ctrl Pts',(1.41747599318129,-0.473000921064237,3.01269480438575));
#5611=CARTESIAN_POINT('Ctrl Pts',(1.29873656917601,-0.473287797471458,3.02588334070706));
#5612=CARTESIAN_POINT('Ctrl Pts',(1.17260477262759,-0.497030428020274,3.03726209636996));
#5613=CARTESIAN_POINT('Ctrl Pts',(0.940241249793305,-0.59345255952946,3.05235989856664));
#5614=CARTESIAN_POINT('Ctrl Pts',(0.834013199901827,-0.666140770092873,
3.05607990145755));
#5615=CARTESIAN_POINT('Ctrl Pts',(0.750076984997382,-0.75007698499732,3.05607990145755));
#5616=CARTESIAN_POINT('Ctrl Pts',(0.666140770092937,-0.834013199901768,
3.05607990145755));
#5617=CARTESIAN_POINT('Ctrl Pts',(0.593452559529527,-0.940241249793248,
3.05235989856665));
#5618=CARTESIAN_POINT('Ctrl Pts',(0.497030428020347,-1.17260477262754,3.03726209636996));
#5619=CARTESIAN_POINT('Ctrl Pts',(0.473287797471535,-1.29873656917595,3.02588334070706));
#5620=CARTESIAN_POINT('Ctrl Pts',(0.473000921064317,-1.41747599318107,3.01269480438577));
#5621=CARTESIAN_POINT('Ctrl Pts',(0.472999999999865,-1.4182378430628,3.01261008153858));
#5622=CARTESIAN_POINT('Ctrl Pts',(0.472999999999865,-1.41899999999981,3.01252522110192));
#5623=CARTESIAN_POINT('',(0.651395808575106,-0.866098738193356,0.27));
#5624=CARTESIAN_POINT('Origin',(1.41899999999987,-1.41899999999979,0.27));
#5625=CARTESIAN_POINT('',(0.472999999999865,-1.41899999999981,1.22765307701772));
#5626=CARTESIAN_POINT('Origin',(1.41899999999987,-1.41899999999979,1.22765307701768));
#5627=CARTESIAN_POINT('',(0.472999999999865,-1.41899999999981,3.1));
#5628=CARTESIAN_POINT('Origin',(0.472999999999839,-0.472999999999785,3.1));
#5629=CARTESIAN_POINT('',(0.472999999999892,-2.36767196216382,2.87080111520185));
#5630=CARTESIAN_POINT('Origin',(0.472999999999825,1.32935445800918E-14,
-9.73193776093083));
#5631=CARTESIAN_POINT('',(0.472999999999889,-2.24662499999997,2.66114162663219));
#5632=CARTESIAN_POINT('Origin',(-2.5,0.472999999999654,3.1));
#5633=CARTESIAN_POINT('',(-2.36767196216383,0.472999999999654,2.87080111520186));
#5634=CARTESIAN_POINT('Origin',(8.32667268468867E-16,0.472999999999654,
-9.73193776093083));
#5635=CARTESIAN_POINT('',(-2.5,0.472999999999654,3.1));
#5636=CARTESIAN_POINT('Origin',(-2.5,-0.472999999999893,3.1));
#5637=CARTESIAN_POINT('',(-2.37229341204248,-2.90522153369617E-16,2.87880570119631));
#5638=CARTESIAN_POINT('Origin',(3.68139204037345,0.,-7.60648507542867));
#5639=CARTESIAN_POINT('',(-0.866098738193358,-0.236499999999945,0.27));
#5640=CARTESIAN_POINT('Origin',(3.68139204037345,0.,-7.60648507542867));
#5641=CARTESIAN_POINT('Origin',(-0.472999999999788,-2.5,3.1));
#5642=CARTESIAN_POINT('',(-0.472999999999788,-2.36767196216382,2.87080111520185));
#5643=CARTESIAN_POINT('Origin',(-0.472999999999779,1.82968396778355E-15,
-9.73193776093083));
#5644=CARTESIAN_POINT('',(-0.472999999999788,-2.5,3.1));
#5645=CARTESIAN_POINT('Origin',(0.472999999999896,-2.5,3.1));
#5646=CARTESIAN_POINT('Origin',(6.23325686399709E-15,3.68139204037346,-7.60648507542867));
#5647=CARTESIAN_POINT('',(0.236499999999949,-0.866098738193356,0.27));
#5648=CARTESIAN_POINT('Origin',(1.11022302462516E-15,3.88578058618805E-15,
0.27));
#5649=CARTESIAN_POINT('Origin',(0.,0.,-0.2));
#5650=CARTESIAN_POINT('',(2.37846096908266,-2.91277461268399E-16,-3.46944695195361E-17));
#5651=CARTESIAN_POINT('Origin',(0.,0.,-3.46944695195361E-17));
#5652=CARTESIAN_POINT('',(2.17846096908266,-2.66784525285452E-16,-0.2));
#5653=CARTESIAN_POINT('Origin',(2.37846096908266,-2.91277461268399E-16,
-0.2));
#5654=CARTESIAN_POINT('Origin',(0.,0.,-0.2));
#5655=CARTESIAN_POINT('Origin',(-2.17846096908266,0.,-1.88141750998334E-17));
#5656=CARTESIAN_POINT('',(5.15,-6.30693101560887E-16,-2.77555756156289E-16));
#5657=CARTESIAN_POINT('Origin',(0.,0.,0.));
#5658=CARTESIAN_POINT('Origin',(0.,0.,-0.149999999999999));
#5659=CARTESIAN_POINT('',(2.17846096908266,-2.66784525285452E-16,-0.299999999999998));
#5660=CARTESIAN_POINT('Origin',(0.,0.,-0.299999999999998));
#5661=CARTESIAN_POINT('',(2.17846096908266,-2.66784525285452E-16,-0.149999999999999));
#5662=CARTESIAN_POINT('Origin',(0.,0.,-0.899999999999999));
#5663=CARTESIAN_POINT('',(2.4505,-3.00099698131059E-16,-1.31526348502534));
#5664=CARTESIAN_POINT('Origin',(0.,0.,-1.31526348502534));
#5665=CARTESIAN_POINT('',(2.33923048454133,-2.86473112536145E-16,-0.899999999999999));
#5666=CARTESIAN_POINT('Origin',(0.,0.,-7.75));
#5667=CARTESIAN_POINT('',(2.4505,3.00099698131059E-16,-14.));
#5668=CARTESIAN_POINT('Origin',(0.,0.,-14.));
#5669=CARTESIAN_POINT('',(2.4505,-3.00099698131059E-16,-7.75));
#5670=CARTESIAN_POINT('Origin',(0.,0.,-14.));
#5671=CARTESIAN_POINT('Origin',(8.32667268468867E-16,0.,-9.73193776093083));
#5672=CARTESIAN_POINT('',(-4.96627380657387,0.,2.1));
#5673=CARTESIAN_POINT('Origin',(8.32667268468867E-16,0.,-9.73193776093083));
#5674=CARTESIAN_POINT('',(4.96627380657386,-6.08193132091002E-16,2.1));
#5675=CARTESIAN_POINT('Origin',(0.,0.,2.1));
#5676=CARTESIAN_POINT('Origin',(0.,0.,2.1));
#5677=CARTESIAN_POINT('Origin',(0.,0.,1.05));
#5678=CARTESIAN_POINT('',(5.05813690328693,-6.19443116825945E-16,1.05));
#5679=CARTESIAN_POINT('',(0.,0.,0.));
#5680=CARTESIAN_POINT('Origin',(29.1374542444053,4.,6.));
#5681=CARTESIAN_POINT('',(29.6374542444053,4.,0.));
#5682=CARTESIAN_POINT('',(29.6374542444053,4.,6.));
#5683=CARTESIAN_POINT('',(29.6374542444053,4.,11.));
#5684=CARTESIAN_POINT('',(35.1374542444053,4.,0.));
#5685=CARTESIAN_POINT('',(14.5687271222026,4.,0.));
#5686=CARTESIAN_POINT('',(35.1374542444053,4.,6.));
#5687=CARTESIAN_POINT('',(35.1374542444053,4.,6.));
#5688=CARTESIAN_POINT('',(29.1374542444053,4.,6.));
#5689=CARTESIAN_POINT('Origin',(29.1374542444053,-4.,6.));
#5690=CARTESIAN_POINT('',(29.6374542444053,-4.,6.));
#5691=CARTESIAN_POINT('',(29.6374542444053,13.,6.));
#5692=CARTESIAN_POINT('',(35.1374542444053,-4.,6.));
#5693=CARTESIAN_POINT('',(35.1374542444053,-4.,6.));
#5694=CARTESIAN_POINT('',(29.1374542444053,-4.,6.));
#5695=CARTESIAN_POINT('Origin',(29.1374542444053,-4.,0.));
#5696=CARTESIAN_POINT('',(29.6374542444053,-4.,0.));
#5697=CARTESIAN_POINT('',(29.6374542444053,-4.,8.));
#5698=CARTESIAN_POINT('',(35.1374542444053,-4.,0.));
#5699=CARTESIAN_POINT('',(35.1374542444053,-4.,-6.));
#5700=CARTESIAN_POINT('',(14.5687271222026,-4.,0.));
#5701=CARTESIAN_POINT('Origin',(35.1374542444053,0.,3.));
#5702=CARTESIAN_POINT('',(35.1374542444053,0.,0.));
#5703=CARTESIAN_POINT('Origin',(0.,0.,0.));
#5704=CARTESIAN_POINT('',(29.6374542444053,30.,0.));
#5705=CARTESIAN_POINT('',(29.6374542444053,15.,0.));
#5706=CARTESIAN_POINT('',(50.,30.,0.));
#5707=CARTESIAN_POINT('',(-50.,30.,0.));
#5708=CARTESIAN_POINT('',(50.,-30.,0.));
#5709=CARTESIAN_POINT('',(50.,30.,0.));
#5710=CARTESIAN_POINT('',(29.6374542444053,-30.,0.));
#5711=CARTESIAN_POINT('',(50.,-30.,0.));
#5712=CARTESIAN_POINT('',(29.6374542444053,15.,0.));
#5713=CARTESIAN_POINT('',(44.5175,22.,0.));
#5714=CARTESIAN_POINT('Origin',(42.,22.,0.));
#5715=CARTESIAN_POINT('',(44.5175,-22.,0.));
#5716=CARTESIAN_POINT('Origin',(42.,-22.,0.));
#5717=CARTESIAN_POINT('Origin',(29.6374542444053,30.,16.));
#5718=CARTESIAN_POINT('',(29.6374542444053,-30.,16.));
#5719=CARTESIAN_POINT('',(29.6374542444053,-30.,8.));
#5720=CARTESIAN_POINT('',(29.6374542444053,30.,16.));
#5721=CARTESIAN_POINT('',(29.6374542444053,15.,16.));
#5722=CARTESIAN_POINT('',(29.6374542444053,30.,8.));
#5723=CARTESIAN_POINT('Origin',(0.,0.,16.));
#5724=CARTESIAN_POINT('',(50.,-30.,16.));
#5725=CARTESIAN_POINT('',(50.,-30.,16.));
#5726=CARTESIAN_POINT('',(50.,30.,16.));
#5727=CARTESIAN_POINT('',(50.,30.,16.));
#5728=CARTESIAN_POINT('',(-50.,30.,16.));
#5729=CARTESIAN_POINT('',(44.5175,-22.,16.));
#5730=CARTESIAN_POINT('Origin',(42.,-22.,16.));
#5731=CARTESIAN_POINT('',(44.5175,22.,16.));
#5732=CARTESIAN_POINT('Origin',(42.,22.,16.));
#5733=CARTESIAN_POINT('Origin',(-50.,-30.,0.));
#5734=CARTESIAN_POINT('',(50.,-30.,0.));
#5735=CARTESIAN_POINT('Origin',(50.,30.,0.));
#5736=CARTESIAN_POINT('',(50.,30.,0.));
#5737=CARTESIAN_POINT('Origin',(42.,22.,16.));
#5738=CARTESIAN_POINT('',(44.5175,22.,16.));
#5739=CARTESIAN_POINT('Origin',(42.,-22.,16.));
#5740=CARTESIAN_POINT('',(44.5175,-22.,16.));
#5741=CARTESIAN_POINT('Origin',(50.,-30.,0.));
#5742=CARTESIAN_POINT('',(0.,0.,0.));
#5743=CARTESIAN_POINT('Origin',(-29.1374542444053,4.,6.));
#5744=CARTESIAN_POINT('',(-29.1374542444053,4.,0.));
#5745=CARTESIAN_POINT('',(-29.1374542444053,4.,6.));
#5746=CARTESIAN_POINT('',(-29.1374542444053,4.,11.));
#5747=CARTESIAN_POINT('',(-35.1374542444053,4.,0.));
#5748=CARTESIAN_POINT('',(-29.1374542444053,4.,0.));
#5749=CARTESIAN_POINT('',(-35.1374542444053,4.,6.));
#5750=CARTESIAN_POINT('',(-35.1374542444053,4.,6.));
#5751=CARTESIAN_POINT('',(-29.1374542444053,4.,6.));
#5752=CARTESIAN_POINT('Origin',(-29.1374542444053,-4.,6.));
#5753=CARTESIAN_POINT('',(-29.1374542444053,-4.,6.));
#5754=CARTESIAN_POINT('',(-29.1374542444053,13.,6.));
#5755=CARTESIAN_POINT('',(-35.1374542444053,-4.,6.));
#5756=CARTESIAN_POINT('',(-35.1374542444053,-4.,6.));
#5757=CARTESIAN_POINT('',(-29.1374542444053,-4.,6.));
#5758=CARTESIAN_POINT('Origin',(-29.1374542444053,-4.,0.));
#5759=CARTESIAN_POINT('',(-29.1374542444053,-4.,0.));
#5760=CARTESIAN_POINT('',(-29.1374542444053,-4.,8.));
#5761=CARTESIAN_POINT('',(-35.1374542444053,-4.,0.));
#5762=CARTESIAN_POINT('',(-35.1374542444053,-4.,-6.));
#5763=CARTESIAN_POINT('',(-29.1374542444053,-4.,0.));
#5764=CARTESIAN_POINT('Origin',(-35.1374542444053,0.,3.));
#5765=CARTESIAN_POINT('',(-35.1374542444053,30.,0.));
#5766=CARTESIAN_POINT('Origin',(-29.1374542444053,30.,16.));
#5767=CARTESIAN_POINT('',(-29.1374542444053,-30.,0.));
#5768=CARTESIAN_POINT('',(-29.1374542444053,15.,0.));
#5769=CARTESIAN_POINT('',(-29.1374542444053,-30.,16.));
#5770=CARTESIAN_POINT('',(-29.1374542444053,-30.,8.));
#5771=CARTESIAN_POINT('',(-29.1374542444053,30.,16.));
#5772=CARTESIAN_POINT('',(-29.1374542444053,15.,16.));
#5773=CARTESIAN_POINT('',(-29.1374542444053,30.,0.));
#5774=CARTESIAN_POINT('',(-29.1374542444053,30.,8.));
#5775=CARTESIAN_POINT('',(-29.1374542444053,15.,0.));
#5776=CARTESIAN_POINT('Origin',(-11.6523566026163,-30.,8.));
#5777=CARTESIAN_POINT('',(-14.1523566026163,15.,8.));
#5778=CARTESIAN_POINT('Origin',(-11.6523566026163,15.,8.));
#5779=CARTESIAN_POINT('',(-14.1523566026163,30.,8.));
#5780=CARTESIAN_POINT('',(-14.1523566026163,-30.,8.));
#5781=CARTESIAN_POINT('Origin',(-11.6523566026163,30.,8.));
#5782=CARTESIAN_POINT('Origin',(-17.8106534302817,8.98579659039556,16.));
#5783=CARTESIAN_POINT('',(-21.,8.98579659039556,0.));
#5784=CARTESIAN_POINT('',(-20.,8.98579659039556,0.));
#5785=CARTESIAN_POINT('',(-8.90532671514083,8.98579659039556,0.));
#5786=CARTESIAN_POINT('',(-21.,8.98579659039556,16.));
#5787=CARTESIAN_POINT('',(-21.,8.98579659039556,16.));
#5788=CARTESIAN_POINT('',(-20.,8.98579659039556,16.));
#5789=CARTESIAN_POINT('',(-8.90532671514083,8.98579659039556,16.));
#5790=CARTESIAN_POINT('',(-20.,8.98579659039556,16.));
#5791=CARTESIAN_POINT('Origin',(-21.,13.1380156428221,16.));
#5792=CARTESIAN_POINT('',(-18.8926671865707,13.1380156428221,0.));
#5793=CARTESIAN_POINT('',(-21.,13.1380156428221,0.));
#5794=CARTESIAN_POINT('',(-10.5,13.1380156428221,0.));
#5795=CARTESIAN_POINT('',(-18.8926671865707,13.1380156428221,16.));
#5796=CARTESIAN_POINT('',(-18.8926671865707,13.1380156428221,16.));
#5797=CARTESIAN_POINT('',(-21.,13.1380156428221,16.));
#5798=CARTESIAN_POINT('',(-10.5,13.1380156428221,16.));
#5799=CARTESIAN_POINT('',(-21.,13.1380156428221,16.));
#5800=CARTESIAN_POINT('Origin',(-21.,8.98579659039556,16.));
#5801=CARTESIAN_POINT('',(-21.,4.49289829519778,0.));
#5802=CARTESIAN_POINT('',(-21.,4.49289829519778,16.));
#5803=CARTESIAN_POINT('Origin',(-20.,-10.,16.));
#5804=CARTESIAN_POINT('',(-20.,-2.10952062437159,16.));
#5805=CARTESIAN_POINT('',(-20.,-5.,16.));
#5806=CARTESIAN_POINT('',(-20.,-2.10952062437159,14.));
#5807=CARTESIAN_POINT('',(-20.,-2.10952062437159,16.));
#5808=CARTESIAN_POINT('',(-20.,-10.,14.));
#5809=CARTESIAN_POINT('',(-20.,-8.5547603121858,14.));
#5810=CARTESIAN_POINT('',(-20.,-10.,0.));
#5811=CARTESIAN_POINT('',(-20.,-10.,16.));
#5812=CARTESIAN_POINT('',(-20.,-5.,0.));
#5813=CARTESIAN_POINT('Origin',(25.,-12.1095206243716,16.));
#5814=CARTESIAN_POINT('',(-19.5332022605826,-12.1095206243716,14.));
#5815=CARTESIAN_POINT('',(-19.5332022605826,-12.1095206243716,16.));
#5816=CARTESIAN_POINT('',(-19.5332022605826,-12.1095206243716,16.));
#5817=CARTESIAN_POINT('',(-25.,-12.1095206243716,14.));
#5818=CARTESIAN_POINT('',(-25.,-12.1095206243716,14.));
#5819=CARTESIAN_POINT('',(-25.,-12.1095206243716,16.));
#5820=CARTESIAN_POINT('',(-25.,-12.1095206243716,16.));
#5821=CARTESIAN_POINT('',(12.5,-12.1095206243716,16.));
#5822=CARTESIAN_POINT('Origin',(-25.,-2.10952062437159,16.));
#5823=CARTESIAN_POINT('',(-25.,-2.10952062437159,16.));
#5824=CARTESIAN_POINT('',(-12.5,-2.10952062437159,16.));
#5825=CARTESIAN_POINT('',(-25.,-2.10952062437159,14.));
#5826=CARTESIAN_POINT('',(-25.,-2.10952062437159,16.));
#5827=CARTESIAN_POINT('',(25.,-2.10952062437159,14.));
#5828=CARTESIAN_POINT('Origin',(-25.,-12.1095206243716,16.));
#5829=CARTESIAN_POINT('',(-25.,-6.0547603121858,16.));
#5830=CARTESIAN_POINT('',(-25.,-2.10952062437159,14.));
#5831=CARTESIAN_POINT('Origin',(0.,-7.10952062437159,14.));
#5832=CARTESIAN_POINT('Origin',(-15.,-10.,14.));
#5833=CARTESIAN_POINT('Origin',(-15.,15.,16.));
#5834=CARTESIAN_POINT('',(-15.,15.,16.));
#5835=CARTESIAN_POINT('',(29.1374542444053,15.,16.));
#5836=CARTESIAN_POINT('',(7.5,15.,16.));
#5837=CARTESIAN_POINT('',(-15.,15.,0.));
#5838=CARTESIAN_POINT('',(-15.,15.,16.));
#5839=CARTESIAN_POINT('',(29.1374542444053,15.,0.));
#5840=CARTESIAN_POINT('',(7.5,15.,0.));
#5841=CARTESIAN_POINT('',(29.1374542444053,15.,16.));
#5842=CARTESIAN_POINT('Origin',(-15.,10.,16.));
#5843=CARTESIAN_POINT('Origin',(-15.,10.,0.));
#5844=CARTESIAN_POINT('Origin',(-15.,10.,16.));
#5845=CARTESIAN_POINT('Origin',(50.,30.,0.));
#5846=CARTESIAN_POINT('',(29.1374542444053,30.,16.));
#5847=CARTESIAN_POINT('',(29.1374542444053,30.,0.));
#5848=CARTESIAN_POINT('',(29.1374542444053,30.,8.));
#5849=CARTESIAN_POINT('',(-50.,30.,0.));
#5850=CARTESIAN_POINT('',(-50.,30.,16.));
#5851=CARTESIAN_POINT('Origin',(0.,0.,0.));
#5852=CARTESIAN_POINT('',(-19.5332022605826,-12.1095206243716,0.));
#5853=CARTESIAN_POINT('',(-19.5332022605826,-30.,0.));
#5854=CARTESIAN_POINT('',(-19.5332022605826,-15.,0.));
#5855=CARTESIAN_POINT('',(50.,-30.,0.));
#5856=CARTESIAN_POINT('',(29.1374542444053,-15.,0.));
#5857=CARTESIAN_POINT('Origin',(-15.,-10.,0.));
#5858=CARTESIAN_POINT('Origin',(29.1374542444053,-30.,16.));
#5859=CARTESIAN_POINT('',(29.1374542444053,-15.,16.));
#5860=CARTESIAN_POINT('Origin',(0.,0.,16.));
#5861=CARTESIAN_POINT('',(-19.5332022605826,-30.,16.));
#5862=CARTESIAN_POINT('',(-19.5332022605826,-15.,16.));
#5863=CARTESIAN_POINT('',(50.,-30.,16.));
#5864=CARTESIAN_POINT('Origin',(-15.,-10.,16.));
#5865=CARTESIAN_POINT('',(-19.5332022605826,-12.1095206243716,16.));
#5866=CARTESIAN_POINT('Origin',(-50.,-30.,0.));
#5867=CARTESIAN_POINT('',(-19.5332022605826,-30.,8.));
#5868=CARTESIAN_POINT('Origin',(-19.5332022605826,-30.,16.));
#5869=CARTESIAN_POINT('',(0.,0.,0.));
#5870=CARTESIAN_POINT('Origin',(-29.1374542444053,-4.,0.));
#5871=CARTESIAN_POINT('',(-29.6374542444053,-4.,0.));
#5872=CARTESIAN_POINT('',(-29.6374542444053,-4.,6.));
#5873=CARTESIAN_POINT('',(-29.6374542444053,-4.,8.));
#5874=CARTESIAN_POINT('',(-35.1374542444053,-4.,0.));
#5875=CARTESIAN_POINT('',(-14.5687271222026,-4.,0.));
#5876=CARTESIAN_POINT('',(-35.1374542444053,-4.,6.));
#5877=CARTESIAN_POINT('',(-35.1374542444053,-4.,-6.));
#5878=CARTESIAN_POINT('',(-29.1374542444053,-4.,6.));
#5879=CARTESIAN_POINT('Origin',(-29.1374542444053,-4.,6.));
#5880=CARTESIAN_POINT('',(-29.6374542444053,4.,6.));
#5881=CARTESIAN_POINT('',(-29.6374542444053,-17.,6.));
#5882=CARTESIAN_POINT('',(-35.1374542444053,4.,6.));
#5883=CARTESIAN_POINT('',(-35.1374542444053,-4.,6.));
#5884=CARTESIAN_POINT('',(-29.1374542444053,4.,6.));
#5885=CARTESIAN_POINT('Origin',(-29.1374542444053,4.,6.));
#5886=CARTESIAN_POINT('',(-29.6374542444053,4.,0.));
#5887=CARTESIAN_POINT('',(-29.6374542444053,4.,11.));
#5888=CARTESIAN_POINT('',(-35.1374542444053,4.,0.));
#5889=CARTESIAN_POINT('',(-35.1374542444053,4.,6.));
#5890=CARTESIAN_POINT('',(-14.5687271222026,4.,0.));
#5891=CARTESIAN_POINT('Origin',(-35.1374542444053,0.,3.));
#5892=CARTESIAN_POINT('',(-35.1374542444053,0.,0.));
#5893=CARTESIAN_POINT('Origin',(-29.6374542444053,-30.,16.));
#5894=CARTESIAN_POINT('',(-29.6374542444053,30.,0.));
#5895=CARTESIAN_POINT('',(-29.6374542444053,-15.,0.));
#5896=CARTESIAN_POINT('',(-29.6374542444053,30.,16.));
#5897=CARTESIAN_POINT('',(-29.6374542444053,30.,8.));
#5898=CARTESIAN_POINT('',(-29.6374542444053,-30.,16.));
#5899=CARTESIAN_POINT('',(-29.6374542444053,-15.,16.));
#5900=CARTESIAN_POINT('',(-29.6374542444053,-30.,0.));
#5901=CARTESIAN_POINT('',(-29.6374542444053,-30.,8.));
#5902=CARTESIAN_POINT('',(-29.6374542444053,-15.,0.));
#5903=CARTESIAN_POINT('Origin',(0.,0.,16.));
#5904=CARTESIAN_POINT('',(-50.,30.,16.));
#5905=CARTESIAN_POINT('',(-50.,30.,16.));
#5906=CARTESIAN_POINT('',(-50.,-30.,16.));
#5907=CARTESIAN_POINT('',(-50.,-30.,16.));
#5908=CARTESIAN_POINT('',(50.,-30.,16.));
#5909=CARTESIAN_POINT('',(-44.5175,-22.,16.));
#5910=CARTESIAN_POINT('Origin',(-42.,-22.,16.));
#5911=CARTESIAN_POINT('',(-44.5175,22.,16.));
#5912=CARTESIAN_POINT('Origin',(-42.,22.,16.));
#5913=CARTESIAN_POINT('Origin',(-50.,-30.,0.));
#5914=CARTESIAN_POINT('',(-50.,-30.,0.));
#5915=CARTESIAN_POINT('',(-50.,-30.,0.));
#5916=CARTESIAN_POINT('',(50.,-30.,0.));
#5917=CARTESIAN_POINT('Origin',(0.,0.,0.));
#5918=CARTESIAN_POINT('',(-50.,30.,0.));
#5919=CARTESIAN_POINT('',(-50.,-30.,0.));
#5920=CARTESIAN_POINT('',(-50.,30.,0.));
#5921=CARTESIAN_POINT('',(-44.5175,-22.,0.));
#5922=CARTESIAN_POINT('Origin',(-42.,-22.,0.));
#5923=CARTESIAN_POINT('',(-44.5175,22.,0.));
#5924=CARTESIAN_POINT('Origin',(-42.,22.,0.));
#5925=CARTESIAN_POINT('Origin',(50.,30.,0.));
#5926=CARTESIAN_POINT('',(-50.,30.,0.));
#5927=CARTESIAN_POINT('Origin',(-42.,22.,16.));
#5928=CARTESIAN_POINT('',(-44.5175,22.,16.));
#5929=CARTESIAN_POINT('Origin',(-42.,-22.,16.));
#5930=CARTESIAN_POINT('',(-44.5175,-22.,16.));
#5931=CARTESIAN_POINT('Origin',(-50.,30.,0.));
#5932=CARTESIAN_POINT('',(0.,0.,0.));
#5933=CARTESIAN_POINT('Origin',(29.1374542444053,4.,6.));
#5934=CARTESIAN_POINT('',(29.1374542444053,4.,6.));
#5935=CARTESIAN_POINT('',(29.1374542444053,4.,0.));
#5936=CARTESIAN_POINT('',(29.1374542444053,4.,11.));
#5937=CARTESIAN_POINT('',(35.1374542444053,4.,6.));
#5938=CARTESIAN_POINT('',(29.1374542444053,4.,6.));
#5939=CARTESIAN_POINT('',(35.1374542444053,4.,0.));
#5940=CARTESIAN_POINT('',(35.1374542444053,4.,6.));
#5941=CARTESIAN_POINT('',(29.1374542444053,4.,0.));
#5942=CARTESIAN_POINT('Origin',(29.1374542444053,-4.,6.));
#5943=CARTESIAN_POINT('',(29.1374542444053,-4.,6.));
#5944=CARTESIAN_POINT('',(29.1374542444053,-17.,6.));
#5945=CARTESIAN_POINT('',(35.1374542444053,-4.,6.));
#5946=CARTESIAN_POINT('',(29.1374542444053,-4.,6.));
#5947=CARTESIAN_POINT('',(35.1374542444053,-4.,6.));
#5948=CARTESIAN_POINT('Origin',(29.1374542444053,-4.,0.));
#5949=CARTESIAN_POINT('',(29.1374542444053,-4.,0.));
#5950=CARTESIAN_POINT('',(29.1374542444053,-4.,8.));
#5951=CARTESIAN_POINT('',(35.1374542444053,-4.,0.));
#5952=CARTESIAN_POINT('',(29.1374542444053,-4.,0.));
#5953=CARTESIAN_POINT('',(35.1374542444053,-4.,-6.));
#5954=CARTESIAN_POINT('Origin',(35.1374542444053,0.,3.));
#5955=CARTESIAN_POINT('',(35.1374542444053,30.,0.));
#5956=CARTESIAN_POINT('Origin',(29.1374542444053,-30.,16.));
#5957=CARTESIAN_POINT('',(29.1374542444053,14.5,0.));
#5958=CARTESIAN_POINT('',(29.1374542444053,-15.,0.));
#5959=CARTESIAN_POINT('',(29.1374542444053,14.5,16.));
#5960=CARTESIAN_POINT('',(29.1374542444053,14.5,16.));
#5961=CARTESIAN_POINT('',(29.1374542444053,-30.,16.));
#5962=CARTESIAN_POINT('',(29.1374542444053,-15.,16.));
#5963=CARTESIAN_POINT('',(29.1374542444053,-30.,0.));
#5964=CARTESIAN_POINT('',(29.1374542444053,-30.,8.));
#5965=CARTESIAN_POINT('',(29.1374542444053,-15.,0.));
#5966=CARTESIAN_POINT('Origin',(-19.0332022605826,-12.9552122639891,16.));
#5967=CARTESIAN_POINT('',(-19.0332022605826,-30.,0.));
#5968=CARTESIAN_POINT('',(-19.0332022605826,-12.9552122639891,0.));
#5969=CARTESIAN_POINT('',(-19.0332022605826,-6.47760613199456,0.));
#5970=CARTESIAN_POINT('',(-19.0332022605826,-30.,16.));
#5971=CARTESIAN_POINT('',(-19.0332022605826,-30.,8.));
#5972=CARTESIAN_POINT('',(-19.0332022605826,-12.9552122639891,16.));
#5973=CARTESIAN_POINT('',(-19.0332022605826,-6.47760613199456,16.));
#5974=CARTESIAN_POINT('',(-19.0332022605826,-12.9552122639891,16.));
#5975=CARTESIAN_POINT('Origin',(29.1374542444053,14.5,16.));
#5976=CARTESIAN_POINT('',(17.1794494717703,14.5,0.));
#5977=CARTESIAN_POINT('',(14.5687271222026,14.5,0.));
#5978=CARTESIAN_POINT('',(17.1794494717703,14.5,16.));
#5979=CARTESIAN_POINT('',(17.1794494717703,14.5,16.));
#5980=CARTESIAN_POINT('',(14.5687271222026,14.5,16.));
#5981=CARTESIAN_POINT('Origin',(-15.,-10.,16.));
#5982=CARTESIAN_POINT('',(-15.,-15.,16.));
#5983=CARTESIAN_POINT('Origin',(-15.,-10.,16.));
#5984=CARTESIAN_POINT('',(-15.,-15.,0.));
#5985=CARTESIAN_POINT('',(-15.,-15.,16.));
#5986=CARTESIAN_POINT('Origin',(-15.,-10.,0.));
#5987=CARTESIAN_POINT('Origin',(0.,0.,0.));
#5988=CARTESIAN_POINT('',(15.,-15.,0.));
#5989=CARTESIAN_POINT('',(7.5,-15.,0.));
#5990=CARTESIAN_POINT('',(20.,-10.,0.));
#5991=CARTESIAN_POINT('Origin',(15.,-10.,0.));
#5992=CARTESIAN_POINT('',(20.,8.18152526714698,0.));
#5993=CARTESIAN_POINT('',(20.,5.,0.));
#5994=CARTESIAN_POINT('',(21.,8.18152526714698,0.));
#5995=CARTESIAN_POINT('',(10.5,8.18152526714698,0.));
#5996=CARTESIAN_POINT('',(21.,12.8450798069859,0.));
#5997=CARTESIAN_POINT('',(21.,6.42253990349293,0.));
#5998=CARTESIAN_POINT('',(19.1116323877362,12.8450798069859,0.));
#5999=CARTESIAN_POINT('',(9.00717937525703,12.8450798069859,0.));
#6000=CARTESIAN_POINT('Origin',(15.,10.,0.));
#6001=CARTESIAN_POINT('',(50.,-30.,0.));
#6002=CARTESIAN_POINT('Origin',(15.,-15.,16.));
#6003=CARTESIAN_POINT('',(15.,-15.,16.));
#6004=CARTESIAN_POINT('',(7.5,-15.,16.));
#6005=CARTESIAN_POINT('',(15.,-15.,16.));
#6006=CARTESIAN_POINT('',(-14.1523566026163,-15.,8.));
#6007=CARTESIAN_POINT('Origin',(-11.6523566026163,-15.,8.));
#6008=CARTESIAN_POINT('Origin',(20.,10.,16.));
#6009=CARTESIAN_POINT('',(20.,8.18152526714698,16.));
#6010=CARTESIAN_POINT('',(20.,8.18152526714698,16.));
#6011=CARTESIAN_POINT('',(20.,-10.,14.));
#6012=CARTESIAN_POINT('',(20.,-10.,16.));
#6013=CARTESIAN_POINT('',(20.,-2.10952062437159,14.));
#6014=CARTESIAN_POINT('',(20.,1.44523968781421,14.));
#6015=CARTESIAN_POINT('',(20.,-2.10952062437159,16.));
#6016=CARTESIAN_POINT('',(20.,-2.10952062437159,16.));
#6017=CARTESIAN_POINT('',(20.,5.,16.));
#6018=CARTESIAN_POINT('Origin',(15.,-10.,16.));
#6019=CARTESIAN_POINT('',(19.5332022605826,-12.1095206243716,16.));
#6020=CARTESIAN_POINT('',(19.5332022605826,-12.1095206243716,14.));
#6021=CARTESIAN_POINT('',(19.5332022605826,-12.1095206243716,16.));
#6022=CARTESIAN_POINT('Origin',(15.,-10.,14.));
#6023=CARTESIAN_POINT('Origin',(15.,-10.,16.));
#6024=CARTESIAN_POINT('Origin',(25.,-2.10952062437159,16.));
#6025=CARTESIAN_POINT('',(25.,-2.10952062437159,16.));
#6026=CARTESIAN_POINT('',(25.,-12.1095206243716,16.));
#6027=CARTESIAN_POINT('',(25.,-1.0547603121858,16.));
#6028=CARTESIAN_POINT('',(25.,-2.10952062437159,14.));
#6029=CARTESIAN_POINT('',(25.,-2.10952062437159,16.));
#6030=CARTESIAN_POINT('',(25.,-12.1095206243716,14.));
#6031=CARTESIAN_POINT('',(25.,-12.1095206243716,14.));
#6032=CARTESIAN_POINT('',(25.,-12.1095206243716,16.));
#6033=CARTESIAN_POINT('Origin',(-25.,-2.10952062437159,16.));
#6034=CARTESIAN_POINT('',(25.,-2.10952062437159,14.));
#6035=CARTESIAN_POINT('',(-12.5,-2.10952062437159,16.));
#6036=CARTESIAN_POINT('Origin',(0.,-7.10952062437159,14.));
#6037=CARTESIAN_POINT('',(-25.,-12.1095206243716,14.));
#6038=CARTESIAN_POINT('Origin',(25.,-12.1095206243716,16.));
#6039=CARTESIAN_POINT('',(12.5,-12.1095206243716,16.));
#6040=CARTESIAN_POINT('Origin',(15.,10.,16.));
#6041=CARTESIAN_POINT('',(19.1116323877362,12.8450798069859,16.));
#6042=CARTESIAN_POINT('',(19.1116323877362,12.8450798069859,16.));
#6043=CARTESIAN_POINT('Origin',(15.,10.,16.));
#6044=CARTESIAN_POINT('Origin',(21.,12.8450798069859,16.));
#6045=CARTESIAN_POINT('',(21.,8.18152526714698,16.));
#6046=CARTESIAN_POINT('',(21.,8.18152526714698,16.));
#6047=CARTESIAN_POINT('',(21.,12.8450798069859,16.));
#6048=CARTESIAN_POINT('',(21.,6.42253990349293,16.));
#6049=CARTESIAN_POINT('',(21.,12.8450798069859,16.));
#6050=CARTESIAN_POINT('Origin',(21.,8.18152526714698,16.));
#6051=CARTESIAN_POINT('',(10.5,8.18152526714698,16.));
#6052=CARTESIAN_POINT('Origin',(18.0143587505141,12.8450798069859,16.));
#6053=CARTESIAN_POINT('',(9.00717937525703,12.8450798069859,16.));
#6054=CARTESIAN_POINT('Origin',(-11.6523566026163,-30.,8.));
#6055=CARTESIAN_POINT('',(-14.1523566026163,-30.,8.));
#6056=CARTESIAN_POINT('Origin',(-11.6523566026163,-30.,8.));
#6057=CARTESIAN_POINT('',(-14.1523566026163,-30.,8.));
#6058=CARTESIAN_POINT('Origin',(-50.,-30.,0.));
#6059=CARTESIAN_POINT('',(50.,-30.,16.));
#6060=CARTESIAN_POINT('Origin',(0.,0.,16.));
#6061=CARTESIAN_POINT('',(0.,0.,0.));
#6062=CARTESIAN_POINT('Ctrl Pts',(-21.,11.5223833765015,10.2662081021742));
#6063=CARTESIAN_POINT('Ctrl Pts',(-20.8245614035088,11.5223833765015,11.0929430110137));
#6064=CARTESIAN_POINT('Ctrl Pts',(-20.4736842105263,11.1043754458166,12.7456006386873));
#6065=CARTESIAN_POINT('Ctrl Pts',(-19.9473684210526,9.37174604195822,14.627693070812));
#6066=CARTESIAN_POINT('Ctrl Pts',(-19.421052631579,6.95264079877442,15.4581010648004));
#6067=CARTESIAN_POINT('Ctrl Pts',(-18.8947368421052,4.4296403847971,15.0371536204255));
#6068=CARTESIAN_POINT('Ctrl Pts',(-18.3684210526316,2.41118846113653,13.4660782459265));
#6069=CARTESIAN_POINT('Ctrl Pts',(-17.8421052631579,1.38370759752575,11.1237050325294));
#6070=CARTESIAN_POINT('Ctrl Pts',(-17.3157894736842,1.59493822839275,8.57461107686665));
#6071=CARTESIAN_POINT('Ctrl Pts',(-16.7894736842105,2.9939316339387,6.43329006745293));
#6072=CARTESIAN_POINT('Ctrl Pts',(-16.2631578947368,5.2434721166514,5.21589900368628));
#6073=CARTESIAN_POINT('Ctrl Pts',(-15.7368421052632,7.80129492555693,5.21589976806491));
#6074=CARTESIAN_POINT('Ctrl Pts',(-15.2105263157895,10.0508340962501,6.43328889288153));
#6075=CARTESIAN_POINT('Ctrl Pts',(-14.6842105263158,11.4498308299117,8.57461329194773));
#6076=CARTESIAN_POINT('Ctrl Pts',(-14.1578947368421,11.6610543305691,11.1237005882441));
#6077=CARTESIAN_POINT('Ctrl Pts',(-13.6315789473684,10.6335882256263,13.4660873044149));
#6078=CARTESIAN_POINT('Ctrl Pts',(-13.1052631578947,8.61510599100168,15.0371350857393));
#6079=CARTESIAN_POINT('Ctrl Pts',(-12.5789473684211,6.09216771054517,15.4581390317312));
#6080=CARTESIAN_POINT('Ctrl Pts',(-12.0526315789474,3.67293400690476,14.6276150452767));
#6081=CARTESIAN_POINT('Ctrl Pts',(-11.5263157894737,1.94056718272496,12.7457630293102));
#6082=CARTESIAN_POINT('Ctrl Pts',(-11.,1.31265859936127,10.2662081017794));
#6083=CARTESIAN_POINT('Ctrl Pts',(-10.4736842105263,1.9405671834026,7.78665317603972));
#6084=CARTESIAN_POINT('Ctrl Pts',(-9.94736842105264,3.67293400518582,5.90480115732107));
#6085=CARTESIAN_POINT('Ctrl Pts',(-9.42105263157895,6.09216771422783,5.07427717605678));
#6086=CARTESIAN_POINT('Ctrl Pts',(-8.89473684210527,8.61510598337903,5.49528111163513));
#6087=CARTESIAN_POINT('Ctrl Pts',(-8.36842105263158,10.6335882412796,7.06632891418456));
#6088=CARTESIAN_POINT('Ctrl Pts',(-7.84210526315789,11.6610542984852,9.40871558692863));
#6089=CARTESIAN_POINT('Ctrl Pts',(-7.31578947368422,11.4498308956436,11.9578029721578));
#6090=CARTESIAN_POINT('Ctrl Pts',(-6.78947368421053,10.0508339615961,14.0991271890608));
#6091=CARTESIAN_POINT('Ctrl Pts',(-6.26315789473684,7.80129520139315,15.3165166870263));
#6092=CARTESIAN_POINT('Ctrl Pts',(-5.73684210526316,5.24347155160944,15.3165166870254));
#6093=CARTESIAN_POINT('Ctrl Pts',(-5.21052631578947,2.99393279140807,14.0991271890622));
#6094=CARTESIAN_POINT('Ctrl Pts',(-4.68421052631579,1.59493585735657,11.9578029721551));
#6095=CARTESIAN_POINT('Ctrl Pts',(-4.15789473684211,1.38371245452358,9.408715586934));
#6096=CARTESIAN_POINT('Ctrl Pts',(-3.63157894736843,2.41117851171133,7.0663289141736));
#6097=CARTESIAN_POINT('Ctrl Pts',(-3.10526315789474,4.42966076964857,5.49528111165755));
#6098=CARTESIAN_POINT('Ctrl Pts',(-2.57894736842106,6.95259903872457,5.07427717601085));
#6099=CARTESIAN_POINT('Ctrl Pts',(-2.05263157894737,9.3718327479206,5.90480115741515));
#6100=CARTESIAN_POINT('Ctrl Pts',(-1.52631578947369,11.1041995693883,7.78665317584699));
#6101=CARTESIAN_POINT('Ctrl Pts',(-1.,11.732108154076,10.2662081021742));
#6102=CARTESIAN_POINT('Ctrl Pts',(-0.47368421052632,11.1041995693883,12.7457630285015));
#6103=CARTESIAN_POINT('Ctrl Pts',(0.052631578947363,9.37183274792061,14.6276150469333));
#6104=CARTESIAN_POINT('Ctrl Pts',(0.578947368421052,6.95259903872456,15.4581390283376));
#6105=CARTESIAN_POINT('Ctrl Pts',(1.10526315789473,4.42966076964857,15.0371350926909));
#6106=CARTESIAN_POINT('Ctrl Pts',(1.63157894736842,2.41117851171132,13.4660872901749));
#6107=CARTESIAN_POINT('Ctrl Pts',(2.1578947368421,1.38371245452358,11.1237006174145));
#6108=CARTESIAN_POINT('Ctrl Pts',(2.68421052631579,1.59493585735657,8.57461323219337));
#6109=CARTESIAN_POINT('Ctrl Pts',(3.21052631578947,2.99393279140808,6.43328901528626));
#6110=CARTESIAN_POINT('Ctrl Pts',(3.73684210526315,5.24347155160942,5.21589951732309));
#6111=CARTESIAN_POINT('Ctrl Pts',(4.26315789473684,7.80129520139315,5.21589951732216));
#6112=CARTESIAN_POINT('Ctrl Pts',(4.78947368421052,10.0508339615961,6.43328901528768));
#6113=CARTESIAN_POINT('Ctrl Pts',(5.31578947368421,11.4498308956436,8.57461323219068));
#6114=CARTESIAN_POINT('Ctrl Pts',(5.84210526315788,11.6610542984852,11.1237006174198));
#6115=CARTESIAN_POINT('Ctrl Pts',(6.36842105263158,10.6335882412796,13.4660872901639));
#6116=CARTESIAN_POINT('Ctrl Pts',(6.89473684210526,8.61510598337902,15.0371350927133));
#6117=CARTESIAN_POINT('Ctrl Pts',(7.42105263157895,6.09216771422785,15.4581390282917));
#6118=CARTESIAN_POINT('Ctrl Pts',(7.94736842105263,3.67293400518582,14.6276150470274));
#6119=CARTESIAN_POINT('Ctrl Pts',(8.47368421052631,1.94056718340261,12.7457630283087));
#6120=CARTESIAN_POINT('Ctrl Pts',(9.,1.31265859936126,10.266208102569));
#6121=CARTESIAN_POINT('Ctrl Pts',(9.52631578947368,1.94056718272496,7.78665317503828));
#6122=CARTESIAN_POINT('Ctrl Pts',(10.0526315789474,3.67293400690476,5.90480115907178));
#6123=CARTESIAN_POINT('Ctrl Pts',(10.578947368421,6.09216771054518,5.07427717261729));
#6124=CARTESIAN_POINT('Ctrl Pts',(11.1052631578947,8.61510599100168,5.49528111860915));
#6125=CARTESIAN_POINT('Ctrl Pts',(11.6315789473684,10.6335882256264,7.06632889993352));
#6126=CARTESIAN_POINT('Ctrl Pts',(12.1578947368421,11.6610543305691,9.40871561610432));
#6127=CARTESIAN_POINT('Ctrl Pts',(12.6842105263158,11.4498308299117,11.9578029124007));
#6128=CARTESIAN_POINT('Ctrl Pts',(13.2105263157895,10.0508340962501,14.0991273114669));
#6129=CARTESIAN_POINT('Ctrl Pts',(13.7368421052632,7.80129492555691,15.3165164362836));
#6130=CARTESIAN_POINT('Ctrl Pts',(14.2631578947369,5.24347211665139,15.3165172006622));
#6131=CARTESIAN_POINT('Ctrl Pts',(14.7894736842105,2.9939316339387,14.0991261368955));
#6132=CARTESIAN_POINT('Ctrl Pts',(15.3157894736842,1.59493822839275,11.9578051274818));
#6133=CARTESIAN_POINT('Ctrl Pts',(15.8421052631579,1.38370759752574,9.4087111718191));
#6134=CARTESIAN_POINT('Ctrl Pts',(16.3684210526316,2.41118846113653,7.06633795842197));
#6135=CARTESIAN_POINT('Ctrl Pts',(16.8947368421052,4.42964038479711,5.49526258392294));
#6136=CARTESIAN_POINT('Ctrl Pts',(17.421052631579,6.95264079877441,5.07431513954803));
#6137=CARTESIAN_POINT('Ctrl Pts',(17.9473684210526,9.37174604195823,5.90472313353644));
#6138=CARTESIAN_POINT('Ctrl Pts',(18.4736842105263,11.1043754458165,7.78681556566119));
#6139=CARTESIAN_POINT('Ctrl Pts',(18.8245614035088,11.5223833765015,9.43947319333481));
#6140=CARTESIAN_POINT('Ctrl Pts',(19.,11.5223833765015,10.2662081021742));
#6141=CARTESIAN_POINT('Ctrl Pts',(-21.,11.2231840761596,10.2662081021742));
#6142=CARTESIAN_POINT('Ctrl Pts',(-20.8245614035088,11.2231840761596,11.0435502111341));
#6143=CARTESIAN_POINT('Ctrl Pts',(-20.4736842105263,10.8302077771026,12.5971984651315));
#6144=CARTESIAN_POINT('Ctrl Pts',(-19.9473684210526,9.20124552415081,14.3667344370862));
#6145=CARTESIAN_POINT('Ctrl Pts',(-19.421052631579,6.92689676613498,15.1474232419311));
#6146=CARTESIAN_POINT('Ctrl Pts',(-18.8947368421052,4.5548634960706,14.7516786250889));
#6147=CARTESIAN_POINT('Ctrl Pts',(-18.3684210526316,2.65719094980127,13.2746048239391));
#6148=CARTESIAN_POINT('Ctrl Pts',(-17.8421052631579,1.69119113188947,11.0723959995552));
#6149=CARTESIAN_POINT('Ctrl Pts',(-17.3157894736842,1.88978255726589,8.67583085991063));
#6150=CARTESIAN_POINT('Ctrl Pts',(-16.7894736842105,3.20506407724957,6.6626412124837));
#6151=CARTESIAN_POINT('Ctrl Pts',(-16.2631578947368,5.31999853405079,5.51809495225076));
#6152=CARTESIAN_POINT('Ctrl Pts',(-15.7368421052632,7.72476850015569,5.51809586750696));
#6153=CARTESIAN_POINT('Ctrl Pts',(-15.2105263157895,9.83970168123886,6.66263980606847));
#6154=CARTESIAN_POINT('Ctrl Pts',(-14.6842105263158,11.1549864372545,8.67583351221754));
#6155=CARTESIAN_POINT('Ctrl Pts',(-14.1578947368421,11.3535709297029,11.0723906780295));
#6156=CARTESIAN_POINT('Ctrl Pts',(-13.6315789473684,10.3875854621103,13.2746156704571));
#6157=CARTESIAN_POINT('Ctrl Pts',(-13.1052631578947,8.48988344353287,14.751656431547));
#6158=CARTESIAN_POINT('Ctrl Pts',(-12.5789473684211,6.11791058785403,15.1474687057993));
#6159=CARTESIAN_POINT('Ctrl Pts',(-12.0526315789474,3.84343692367721,14.36664090272));
#6160=CARTESIAN_POINT('Ctrl Pts',(-11.5263157894737,2.21472998524374,12.5973935404023));
#6161=CARTESIAN_POINT('Ctrl Pts',(-11.,1.62439365922802,10.2662081017015));
#6162=CARTESIAN_POINT('Ctrl Pts',(-10.4736842105263,2.21472998590263,7.93502266514533));
#6163=CARTESIAN_POINT('Ctrl Pts',(-9.94736842105264,3.84343692200583,6.16577529953216));
#6164=CARTESIAN_POINT('Ctrl Pts',(-9.42105263157895,6.11791059143481,5.38494750266754));
#6165=CARTESIAN_POINT('Ctrl Pts',(-8.89473684210527,8.48988343612111,5.78075976445089));
#6166=CARTESIAN_POINT('Ctrl Pts',(-8.36842105263158,10.3875854773305,7.25780055095535));
#6167=CARTESIAN_POINT('Ctrl Pts',(-7.84210526315789,11.3535708985067,9.46002549138446));
#6168=CARTESIAN_POINT('Ctrl Pts',(-7.31578947368422,11.1549865011677,11.8565827636832));
#6169=CARTESIAN_POINT('Ctrl Pts',(-6.78947368421053,9.83970155031053,13.8697762517126));
#6170=CARTESIAN_POINT('Ctrl Pts',(-6.26315789473684,7.72476876835996,15.0143206370773));
#6171=CARTESIAN_POINT('Ctrl Pts',(-5.73684210526316,5.31999798464263,15.0143206370762));
#6172=CARTESIAN_POINT('Ctrl Pts',(-5.21052631578947,3.20506520269362,13.8697762517143));
#6173=CARTESIAN_POINT('Ctrl Pts',(-4.68421052631579,1.88978025183249,11.8565827636799));
#6174=CARTESIAN_POINT('Ctrl Pts',(-4.15789473684211,1.69119585450193,9.4600254913909));
#6175=CARTESIAN_POINT('Ctrl Pts',(-3.63157894736843,2.65718127566077,7.25780055094221));
#6176=CARTESIAN_POINT('Ctrl Pts',(-3.10526315789474,4.55488331690579,5.78075976447775));
#6177=CARTESIAN_POINT('Ctrl Pts',(-2.57894736842106,6.926856161519,5.38494750261254));
#6178=CARTESIAN_POINT('Ctrl Pts',(-2.05263157894737,9.20132983109773,6.16577529964482));
#6179=CARTESIAN_POINT('Ctrl Pts',(-1.52631578947369,10.8300367668942,7.93502266491455));
#6180=CARTESIAN_POINT('Ctrl Pts',(-1.,11.4203730941972,10.2662081021742));
#6181=CARTESIAN_POINT('Ctrl Pts',(-0.47368421052632,10.8300367668942,12.5973935394339));
#6182=CARTESIAN_POINT('Ctrl Pts',(0.052631578947363,9.20132983109773,14.3666409047036));
#6183=CARTESIAN_POINT('Ctrl Pts',(0.578947368421052,6.92685616151899,15.1474687017359));
#6184=CARTESIAN_POINT('Ctrl Pts',(1.10526315789473,4.55488331690579,14.7516564398707));
#6185=CARTESIAN_POINT('Ctrl Pts',(1.63157894736842,2.65718127566077,13.2746156534063));
#6186=CARTESIAN_POINT('Ctrl Pts',(2.1578947368421,1.69119585450193,11.0723907129576));
#6187=CARTESIAN_POINT('Ctrl Pts',(2.68421052631579,1.88978025183249,8.67583344066851));
#6188=CARTESIAN_POINT('Ctrl Pts',(3.21052631578947,3.20506520269362,6.66263995263416));
#6189=CARTESIAN_POINT('Ctrl Pts',(3.73684210526315,5.31999798464262,5.51809556727224));
#6190=CARTESIAN_POINT('Ctrl Pts',(4.26315789473684,7.72476876835996,5.51809556727114));
#6191=CARTESIAN_POINT('Ctrl Pts',(4.78947368421052,9.83970155031051,6.66263995263585));
#6192=CARTESIAN_POINT('Ctrl Pts',(5.31578947368421,11.1549865011677,8.6758334406653));
#6193=CARTESIAN_POINT('Ctrl Pts',(5.84210526315788,11.3535708985067,11.072390712964));
#6194=CARTESIAN_POINT('Ctrl Pts',(6.36842105263158,10.3875854773305,13.2746156533931));
#6195=CARTESIAN_POINT('Ctrl Pts',(6.89473684210526,8.48988343612111,14.7516564398976));
#6196=CARTESIAN_POINT('Ctrl Pts',(7.42105263157895,6.11791059143481,15.1474687016809));
#6197=CARTESIAN_POINT('Ctrl Pts',(7.94736842105263,3.84343692200584,14.3666409048163));
#6198=CARTESIAN_POINT('Ctrl Pts',(8.47368421052631,2.21472998590264,12.5973935392031));
#6199=CARTESIAN_POINT('Ctrl Pts',(9.,1.62439365922802,10.266208102647));
#6200=CARTESIAN_POINT('Ctrl Pts',(9.52631578947368,2.21472998524374,7.9350226639462));
#6201=CARTESIAN_POINT('Ctrl Pts',(10.0526315789474,3.84343692367721,6.16577530162845));
#6202=CARTESIAN_POINT('Ctrl Pts',(10.578947368421,6.11791058785404,5.38494749854914));
#6203=CARTESIAN_POINT('Ctrl Pts',(11.1052631578947,8.48988344353287,5.78075977280148));
#6204=CARTESIAN_POINT('Ctrl Pts',(11.6315789473684,10.3875854621103,7.25780053389135));
#6205=CARTESIAN_POINT('Ctrl Pts',(12.1578947368421,11.3535709297029,9.460025526319));
#6206=CARTESIAN_POINT('Ctrl Pts',(12.6842105263158,11.1549864372545,11.8565826921309));
#6207=CARTESIAN_POINT('Ctrl Pts',(13.2105263157895,9.83970168123886,13.86977639828));
#6208=CARTESIAN_POINT('Ctrl Pts',(13.7368421052632,7.72476850015567,15.0143203368415));
#6209=CARTESIAN_POINT('Ctrl Pts',(14.2631578947369,5.31999853405078,15.0143212520977));
#6210=CARTESIAN_POINT('Ctrl Pts',(14.7894736842105,3.20506407724957,13.8697749918648));
#6211=CARTESIAN_POINT('Ctrl Pts',(15.3157894736842,1.88978255726589,11.8565853444378));
#6212=CARTESIAN_POINT('Ctrl Pts',(15.8421052631579,1.69119113188946,9.46002020479329));
#6213=CARTESIAN_POINT('Ctrl Pts',(16.3684210526316,2.65719094980128,7.25781138040935));
#6214=CARTESIAN_POINT('Ctrl Pts',(16.8947368421052,4.5548634960706,5.78073757925955));
#6215=CARTESIAN_POINT('Ctrl Pts',(17.421052631579,6.92689676613498,5.38499296241738));
#6216=CARTESIAN_POINT('Ctrl Pts',(17.9473684210526,9.20124552415082,6.16568176726222));
#6217=CARTESIAN_POINT('Ctrl Pts',(18.4736842105263,10.8302077771026,7.93521773921696));
#6218=CARTESIAN_POINT('Ctrl Pts',(18.8245614035088,11.2231840761596,9.48886599321435));
#6219=CARTESIAN_POINT('Ctrl Pts',(19.,11.2231840761596,10.2662081021742));
#6220=CARTESIAN_POINT('Ctrl Pts',(-20.7137377535255,10.6269009396766,10.2662081021742));
#6221=CARTESIAN_POINT('Ctrl Pts',(-20.5382991570343,10.6269009396766,10.945005547204));
#6222=CARTESIAN_POINT('Ctrl Pts',(-20.1874219640519,10.2837860836795,12.3014923419689));
#6223=CARTESIAN_POINT('Ctrl Pts',(-19.6611061745782,8.86144321099575,13.8466183137858));
#6224=CARTESIAN_POINT('Ctrl Pts',(-19.1347903851045,6.87558727517881,14.528258281606));
#6225=CARTESIAN_POINT('Ctrl Pts',(-18.6084745956308,4.80443303568469,14.182722745685));
#6226=CARTESIAN_POINT('Ctrl Pts',(-18.0821588061571,3.14747146421383,12.8930030485417));
#6227=CARTESIAN_POINT('Ctrl Pts',(-17.5558430166835,2.3040035227468,10.9701359564965));
#6228=CARTESIAN_POINT('Ctrl Pts',(-17.0295272272098,2.47740479551235,8.87756182299855));
#6229=CARTESIAN_POINT('Ctrl Pts',(-16.5032114377361,3.62584936605174,7.11973580265897));
#6230=CARTESIAN_POINT('Ctrl Pts',(-15.9768956482624,5.47251503489257,6.1203691946193));
#6231=CARTESIAN_POINT('Ctrl Pts',(-15.4505798587887,7.57225197059684,6.12037014070636));
#6232=CARTESIAN_POINT('Ctrl Pts',(-14.924264069315,9.41891649399846,7.11973434886793));
#6233=CARTESIAN_POINT('Ctrl Pts',(-14.3979482798413,10.5673639700999,8.87756456464978));
#6234=CARTESIAN_POINT('Ctrl Pts',(-13.8716324903676,10.7407590179416,10.9701304557117));
#6235=CARTESIAN_POINT('Ctrl Pts',(-13.345316700894,9.89730396131102,12.893014260437));
#6236=CARTESIAN_POINT('Ctrl Pts',(-12.8190009114203,8.2403159273021,14.1826998043253));
#6237=CARTESIAN_POINT('Ctrl Pts',(-12.2926851219466,6.16921593255766,14.528305278591));
#6238=CARTESIAN_POINT('Ctrl Pts',(-11.7663693324729,4.18324784624254,13.8465215654802));
#6239=CARTESIAN_POINT('Ctrl Pts',(-11.2400535429992,2.76113421485637,12.3016943587029));
#6240=CARTESIAN_POINT('Ctrl Pts',(-10.7137377535256,2.24567909126825,10.2662081016856));
#6241=CARTESIAN_POINT('Ctrl Pts',(-10.1874219640519,2.76113421544797,8.23072184688508));
#6242=CARTESIAN_POINT('Ctrl Pts',(-9.66110617457818,4.18324784474184,6.68589463670139));
#6243=CARTESIAN_POINT('Ctrl Pts',(-9.1347903851045,6.16921593577276,6.00411093001461));
#6244=CARTESIAN_POINT('Ctrl Pts',(-8.60847459563081,8.24031592064724,6.34971639139128));
#6245=CARTESIAN_POINT('Ctrl Pts',(-8.08215880615713,9.89730397497684,7.63940196155027));
#6246=CARTESIAN_POINT('Ctrl Pts',(-7.55584301668345,10.7407589899312,9.56228571252539));
#6247=CARTESIAN_POINT('Ctrl Pts',(-7.02952722720977,10.5673640274861,11.6548517136612));
#6248=CARTESIAN_POINT('Ctrl Pts',(-6.50321143773608,9.41891637644079,13.412681703976));
#6249=CARTESIAN_POINT('Ctrl Pts',(-5.9768956482624,7.57225221141156,14.4120463739915));
#6250=CARTESIAN_POINT('Ctrl Pts',(-5.45057985878871,5.47251454159106,14.4120463739904));
#6251=CARTESIAN_POINT('Ctrl Pts',(-4.92426406931503,3.62585037656322,13.4126817039777));
#6252=CARTESIAN_POINT('Ctrl Pts',(-4.39794827984135,2.47740272551435,11.6548517136579));
#6253=CARTESIAN_POINT('Ctrl Pts',(-3.87163249036766,2.30400776307679,9.56228571253205));
#6254=CARTESIAN_POINT('Ctrl Pts',(-3.34531670089398,3.14746277801559,7.6394019615367));
#6255=CARTESIAN_POINT('Ctrl Pts',(-2.81900091142029,4.80445083237722,6.34971639141904));
#6256=CARTESIAN_POINT('Ctrl Pts',(-2.29268512194661,6.87555081718607,6.00411092995776));
#6257=CARTESIAN_POINT('Ctrl Pts',(-1.76636933247292,8.86151890835144,6.68589463681784));
#6258=CARTESIAN_POINT('Ctrl Pts',(-1.24005354299924,10.2836325373699,8.23072184664655));
#6259=CARTESIAN_POINT('Ctrl Pts',(-0.713737753525556,10.7990876621138,10.2662081021742));
#6260=CARTESIAN_POINT('Ctrl Pts',(-0.187421964051874,10.2836325373699,12.3016943577019));
#6261=CARTESIAN_POINT('Ctrl Pts',(0.338893825421814,8.86151890835145,13.8465215675306));
#6262=CARTESIAN_POINT('Ctrl Pts',(0.865209614895495,6.87555081718605,14.5283052743907));
#6263=CARTESIAN_POINT('Ctrl Pts',(1.39152540436918,4.80445083237721,14.1826998129294));
#6264=CARTESIAN_POINT('Ctrl Pts',(1.91784119384286,3.14746277801558,12.8930142428118));
#6265=CARTESIAN_POINT('Ctrl Pts',(2.44415698331655,2.30400776307679,10.9701304918164));
#6266=CARTESIAN_POINT('Ctrl Pts',(2.97047277279023,2.47740272551435,8.87756449069058));
#6267=CARTESIAN_POINT('Ctrl Pts',(3.49678856226392,3.62585037656322,7.11973450037077));
#6268=CARTESIAN_POINT('Ctrl Pts',(4.0231043517376,5.47251454159105,6.12036983035809));
#6269=CARTESIAN_POINT('Ctrl Pts',(4.54942014121128,7.57225221141157,6.12036983035694));
#6270=CARTESIAN_POINT('Ctrl Pts',(5.07573593068497,9.41891637644078,7.11973450037252));
#6271=CARTESIAN_POINT('Ctrl Pts',(5.60205172015865,10.5673640274861,8.87756449068726));
#6272=CARTESIAN_POINT('Ctrl Pts',(6.12836750963234,10.7407589899312,10.9701304918231));
#6273=CARTESIAN_POINT('Ctrl Pts',(6.65468329910602,9.89730397497684,12.8930142427982));
#6274=CARTESIAN_POINT('Ctrl Pts',(7.18099908857971,8.24031592064724,14.1826998129572));
#6275=CARTESIAN_POINT('Ctrl Pts',(7.70731487805339,6.16921593577277,14.5283052743338));
#6276=CARTESIAN_POINT('Ctrl Pts',(8.23363066752707,4.18324784474184,13.8465215676471));
#6277=CARTESIAN_POINT('Ctrl Pts',(8.75994645700076,2.76113421544798,12.3016943574634));
#6278=CARTESIAN_POINT('Ctrl Pts',(9.28626224647444,2.24567909126825,10.2662081026629));
#6279=CARTESIAN_POINT('Ctrl Pts',(9.81257803594813,2.76113421485637,8.23072184564557));
#6280=CARTESIAN_POINT('Ctrl Pts',(10.3388938254218,4.18324784624253,6.68589463886829));
#6281=CARTESIAN_POINT('Ctrl Pts',(10.8652096148955,6.16921593255766,6.00411092575748));
#6282=CARTESIAN_POINT('Ctrl Pts',(11.3915254043692,8.24031592730209,6.34971640002317));
#6283=CARTESIAN_POINT('Ctrl Pts',(11.9178411938429,9.89730396131102,7.63940194391146));
#6284=CARTESIAN_POINT('Ctrl Pts',(12.4441569833166,10.7407590179416,9.56228574863674));
#6285=CARTESIAN_POINT('Ctrl Pts',(12.9704727727902,10.5673639700999,11.6548516396987));
#6286=CARTESIAN_POINT('Ctrl Pts',(13.4967885622639,9.41891649399846,13.4126818554805));
#6287=CARTESIAN_POINT('Ctrl Pts',(14.0231043517376,7.57225197059683,14.4120460636421));
#6288=CARTESIAN_POINT('Ctrl Pts',(14.5494201412113,5.47251503489256,14.4120470097292));
#6289=CARTESIAN_POINT('Ctrl Pts',(15.075735930685,3.62584936605174,13.4126804016895));
#6290=CARTESIAN_POINT('Ctrl Pts',(15.6020517201587,2.47740479551235,11.6548543813499));
#6291=CARTESIAN_POINT('Ctrl Pts',(16.1283675096323,2.3040035227468,9.56228024785199));
#6292=CARTESIAN_POINT('Ctrl Pts',(16.654683299106,3.14747146421384,7.63941315580675));
#6293=CARTESIAN_POINT('Ctrl Pts',(17.1809990885797,4.8044330356847,6.34969345866343));
#6294=CARTESIAN_POINT('Ctrl Pts',(17.7073148780534,6.87558727517879,6.00415792274244));
#6295=CARTESIAN_POINT('Ctrl Pts',(18.2336306675271,8.86144321099575,6.68579789056262));
#6296=CARTESIAN_POINT('Ctrl Pts',(18.7599464570008,10.2837860836795,8.2309238623796));
#6297=CARTESIAN_POINT('Ctrl Pts',(19.1108236499832,10.6269009396766,9.58741065714448));
#6298=CARTESIAN_POINT('Ctrl Pts',(19.2862622464744,10.6269009396766,10.2662081021742));
#6299=CARTESIAN_POINT('Ctrl Pts',(-19.7457114929758,10.4071350764215,10.2662081021742));
#6300=CARTESIAN_POINT('Ctrl Pts',(-19.5702728964846,10.4071350764215,10.9084043652423));
#6301=CARTESIAN_POINT('Ctrl Pts',(-19.2193957035022,10.0823325493499,12.1926343284582));
#6302=CARTESIAN_POINT('Ctrl Pts',(-18.6930799140285,8.73618816242606,13.6548102650382));
#6303=CARTESIAN_POINT('Ctrl Pts',(-18.1667641245548,6.85666770773358,14.3000436650509));
#6304=CARTESIAN_POINT('Ctrl Pts',(-17.6404483350811,4.89643689599662,13.9729653727187));
#6305=CARTESIAN_POINT('Ctrl Pts',(-17.1141325456074,3.32820773301878,12.7523373600644));
#6306=CARTESIAN_POINT('Ctrl Pts',(-16.5878167561337,2.52991174299703,10.9324346770084));
#6307=CARTESIAN_POINT('Ctrl Pts',(-16.06150096666,2.6940260673621,8.95193006946043));
#6308=CARTESIAN_POINT('Ctrl Pts',(-15.5351851771864,3.78096813308012,7.28823856150342));
#6309=CARTESIAN_POINT('Ctrl Pts',(-15.0088693877127,5.52873877803479,6.34239253706168));
#6310=CARTESIAN_POINT('Ctrl Pts',(-14.482553598239,7.5160281836638,6.34239279277549));
#6311=CARTESIAN_POINT('Ctrl Pts',(-13.9562378087653,9.26379788184228,7.2882381685645));
#6312=CARTESIAN_POINT('Ctrl Pts',(-13.4299220192916,10.3507423491866,8.95193081048946));
#6313=CARTESIAN_POINT('Ctrl Pts',(-12.9036062298179,10.514851528268,10.9324331902276));
#6314=CARTESIAN_POINT('Ctrl Pts',(-12.3772904403443,9.71656618835865,12.7523403904543));
#6315=CARTESIAN_POINT('Ctrl Pts',(-11.8509746508706,8.14831515246027,13.9729591727957));
#6316=CARTESIAN_POINT('Ctrl Pts',(-11.3246588613969,6.18812917735599,14.3000563616202));
#6317=CARTESIAN_POINT('Ctrl Pts',(-10.7983430719232,4.30851602335673,13.6547843477414));
#6318=CARTESIAN_POINT('Ctrl Pts',(-10.2720272824495,2.96256111851024,12.1926875689854));
#6319=CARTESIAN_POINT('Ctrl Pts',(-9.74571149297584,2.47471026267615,10.2662081020422));
#6320=CARTESIAN_POINT('Ctrl Pts',(-9.21939570350214,2.96256111899924,8.33972863569814));
#6321=CARTESIAN_POINT('Ctrl Pts',(-8.69307991402848,4.30851602211631,6.87763185602132));
#6322=CARTESIAN_POINT('Ctrl Pts',(-8.16676412455478,6.18812918001347,6.23235984387893));
#6323=CARTESIAN_POINT('Ctrl Pts',(-7.64044833508111,8.14831514695963,6.55945702921968));
#6324=CARTESIAN_POINT('Ctrl Pts',(-7.11413254560742,9.7165661996543,7.78007581866172));
#6325=CARTESIAN_POINT('Ctrl Pts',(-6.58781675613373,10.5148515051157,9.59998300436044));
#6326=CARTESIAN_POINT('Ctrl Pts',(-6.06150096666004,10.3507423966199,11.58048541385));
#6327=CARTESIAN_POINT('Ctrl Pts',(-5.53518517718637,9.26379778467361,13.2441779948344));
#6328=CARTESIAN_POINT('Ctrl Pts',(-5.00886938771268,7.51602838271203,14.190023495456));
#6329=CARTESIAN_POINT('Ctrl Pts',(-4.482553598239,5.52873837029065,14.1900234954557));
#6330=CARTESIAN_POINT('Ctrl Pts',(-3.95623780876531,3.78096896833021,13.2441779948349));
#6331=CARTESIAN_POINT('Ctrl Pts',(-3.42992201929163,2.69402435638103,11.5804854138491));
#6332=CARTESIAN_POINT('Ctrl Pts',(-2.90360622981794,2.52991524789141,9.59998300436223));
#6333=CARTESIAN_POINT('Ctrl Pts',(-2.37729044034426,3.32820055333996,7.78007581865805));
#6334=CARTESIAN_POINT('Ctrl Pts',(-1.85097465087057,4.8964516060611,6.55945702922718));
#6335=CARTESIAN_POINT('Ctrl Pts',(-1.32465886139689,6.856637572953,6.23235984386357));
#6336=CARTESIAN_POINT('Ctrl Pts',(-0.798343071923207,8.7362507309613,6.8776318560528));
#6337=CARTESIAN_POINT('Ctrl Pts',(-0.272027282449524,10.0822056338507,8.33972863563365));
#6338=CARTESIAN_POINT('Ctrl Pts',(0.254288507024159,10.5700564906402,10.2662081021742));
#6339=CARTESIAN_POINT('Ctrl Pts',(0.780604296497844,10.0822056338507,12.1926875687148));
#6340=CARTESIAN_POINT('Ctrl Pts',(1.30692008597153,8.73625073096131,13.6547843482957));
#6341=CARTESIAN_POINT('Ctrl Pts',(1.83323587544521,6.85663757295299,14.3000563604849));
#6342=CARTESIAN_POINT('Ctrl Pts',(2.3595516649189,4.8964516060611,13.9729591751213));
#6343=CARTESIAN_POINT('Ctrl Pts',(2.88586745439258,3.32820055333996,12.7523403856904));
#6344=CARTESIAN_POINT('Ctrl Pts',(3.41218324386627,2.52991524789141,10.9324331999862));
#6345=CARTESIAN_POINT('Ctrl Pts',(3.93849903333995,2.69402435638102,8.95193079049936));
#6346=CARTESIAN_POINT('Ctrl Pts',(4.46481482281363,3.78096896833022,7.28823820951355));
#6347=CARTESIAN_POINT('Ctrl Pts',(4.99113061228732,5.52873837029065,6.34239270889278));
#6348=CARTESIAN_POINT('Ctrl Pts',(5.517446401761,7.51602838271202,6.34239270889247));
#6349=CARTESIAN_POINT('Ctrl Pts',(6.04376219123469,9.2637977846736,7.28823820951402));
#6350=CARTESIAN_POINT('Ctrl Pts',(6.57007798070837,10.3507423966199,8.95193079049845));
#6351=CARTESIAN_POINT('Ctrl Pts',(7.09639377018205,10.5148515051157,10.932433199988));
#6352=CARTESIAN_POINT('Ctrl Pts',(7.62270955965573,9.7165661996543,12.7523403856867));
#6353=CARTESIAN_POINT('Ctrl Pts',(8.14902534912942,8.14831514695962,13.9729591751288));
#6354=CARTESIAN_POINT('Ctrl Pts',(8.67534113860311,6.18812918001348,14.3000563604695));
#6355=CARTESIAN_POINT('Ctrl Pts',(9.20165692807679,4.30851602211632,13.6547843483271));
#6356=CARTESIAN_POINT('Ctrl Pts',(9.72797271755048,2.96256111899924,12.1926875686503));
#6357=CARTESIAN_POINT('Ctrl Pts',(10.2542885070242,2.47471026267615,10.2662081023063));
#6358=CARTESIAN_POINT('Ctrl Pts',(10.7806042964978,2.96256111851024,8.33972863536311));
#6359=CARTESIAN_POINT('Ctrl Pts',(11.3069200859715,4.30851602335673,6.877631856607));
#6360=CARTESIAN_POINT('Ctrl Pts',(11.8332358754452,6.18812917735599,6.23235984272829));
#6361=CARTESIAN_POINT('Ctrl Pts',(12.3595516649189,8.14831515246027,6.55945703155276));
#6362=CARTESIAN_POINT('Ctrl Pts',(12.8858674543926,9.71656618835865,7.7800758138942));
#6363=CARTESIAN_POINT('Ctrl Pts',(13.4121832438663,10.514851528268,9.59998301412081));
#6364=CARTESIAN_POINT('Ctrl Pts',(13.9384990333399,10.3507423491866,11.580485393859));
#6365=CARTESIAN_POINT('Ctrl Pts',(14.4648148228136,9.26379788184228,13.244178035784));
#6366=CARTESIAN_POINT('Ctrl Pts',(14.9911306122873,7.51602818366379,14.190023411573));
#6367=CARTESIAN_POINT('Ctrl Pts',(15.517446401761,5.52873877803478,14.1900236672868));
#6368=CARTESIAN_POINT('Ctrl Pts',(16.0437621912347,3.78096813308012,13.244177642845));
#6369=CARTESIAN_POINT('Ctrl Pts',(16.5700779807084,2.6940260673621,11.580486134888));
#6370=CARTESIAN_POINT('Ctrl Pts',(17.0963937701821,2.52991174299704,9.59998152734011));
#6371=CARTESIAN_POINT('Ctrl Pts',(17.6227095596557,3.32820773301878,7.78007884428401));
#6372=CARTESIAN_POINT('Ctrl Pts',(18.1490253491294,4.89643689599663,6.55945083162973));
#6373=CARTESIAN_POINT('Ctrl Pts',(18.6753411386031,6.85666770773357,6.23237253929761));
#6374=CARTESIAN_POINT('Ctrl Pts',(19.2016569280768,8.73618816242606,6.87760593931028));
#6375=CARTESIAN_POINT('Ctrl Pts',(19.7279727175505,10.0823325493499,8.3397818758903));
#6376=CARTESIAN_POINT('Ctrl Pts',(20.0788499105329,10.4071350764215,9.62401183910617));
#6377=CARTESIAN_POINT('Ctrl Pts',(20.2542885070242,10.4071350764215,10.2662081021742));
#6378=CARTESIAN_POINT('Ctrl Pts',(-18.9673979627111,11.0253866956159,10.2662081021742));
#6379=CARTESIAN_POINT('Ctrl Pts',(-18.7919593662199,11.0253866956159,11.0108242444962));
#6380=CARTESIAN_POINT('Ctrl Pts',(-18.4410821732374,10.648941808576,12.499124383921));
#6381=CARTESIAN_POINT('Ctrl Pts',(-17.9147663837637,9.08852492824315,14.1941879499634));
#6382=CARTESIAN_POINT('Ctrl Pts',(-17.3884505942901,6.90987534694561,14.9420335378486));
#6383=CARTESIAN_POINT('Ctrl Pts',(-16.8621348048164,4.63765298021549,14.5629378567814));
#6384=CARTESIAN_POINT('Ctrl Pts',(-16.3358190153427,2.8198305198544,13.1480179635823));
#6385=CARTESIAN_POINT('Ctrl Pts',(-15.809503225869,1.89447816606942,11.0384729586759));
#6386=CARTESIAN_POINT('Ctrl Pts',(-15.2831874363953,2.08471320623785,8.74275090650475));
#6387=CARTESIAN_POINT('Ctrl Pts',(-14.7568716469216,3.3446503103771,6.81427210911637));
#6388=CARTESIAN_POINT('Ctrl Pts',(-14.2305558574479,5.3705925024193,5.71788617736171));
#6389=CARTESIAN_POINT('Ctrl Pts',(-13.7042400679743,7.67417451789751,5.71788701062985));
#6390=CARTESIAN_POINT('Ctrl Pts',(-13.1779242785006,9.70011549723399,6.81427082868689));
#6391=CARTESIAN_POINT('Ctrl Pts',(-12.6516084890269,10.9600556775659,8.74275332121974));
#6392=CARTESIAN_POINT('Ctrl Pts',(-12.1252926995532,11.1502841272486,11.0384681138492));
#6393=CARTESIAN_POINT('Ctrl Pts',(-11.5989769100795,10.2249454149688,13.1480278384744));
#6394=CARTESIAN_POINT('Ctrl Pts',(-11.0726611206058,8.40709493804338,14.5629176513865));
#6395=CARTESIAN_POINT('Ctrl Pts',(-10.5463453311322,6.13493000161398,14.9420749286073));
#6396=CARTESIAN_POINT('Ctrl Pts',(-10.0200295416585,3.95616168372213,14.194102813041));
#6397=CARTESIAN_POINT('Ctrl Pts',(-9.49371375218478,2.39598750700088,12.499301874919));
#6398=CARTESIAN_POINT('Ctrl Pts',(-8.96739796271111,1.83049136418784,10.2662081017439));
#6399=CARTESIAN_POINT('Ctrl Pts',(-8.44108217323742,2.39598750762722,8.03311433052112));
#6400=CARTESIAN_POINT('Ctrl Pts',(-7.91476638376373,3.95616168213331,6.33831338939892));
#6401=CARTESIAN_POINT('Ctrl Pts',(-7.38845059429005,6.13493000501789,5.59034127949062));
#6402=CARTESIAN_POINT('Ctrl Pts',(-6.86213480481637,8.40709493099772,5.96949854535944));
#6403=CARTESIAN_POINT('Ctrl Pts',(-6.33581901534268,10.2249454294372,7.38438838140947));
#6404=CARTESIAN_POINT('Ctrl Pts',(-5.809503225869,11.1502840975933,9.49394805869413));
#6405=CARTESIAN_POINT('Ctrl Pts',(-5.28318743639531,10.9600557383222,11.7896629482713));
#6406=CARTESIAN_POINT('Ctrl Pts',(-4.75687164692163,9.70011537277267,13.7181452422236));
#6407=CARTESIAN_POINT('Ctrl Pts',(-4.23055585744794,7.67417477285422,14.8145294670595));
#6408=CARTESIAN_POINT('Ctrl Pts',(-3.70424006797426,5.37059198014839,14.8145294670585));
#6409=CARTESIAN_POINT('Ctrl Pts',(-3.17792427850058,3.3446513802314,13.7181452422251));
#6410=CARTESIAN_POINT('Ctrl Pts',(-2.65160848902689,2.08471101467814,11.7896629482684));
#6411=CARTESIAN_POINT('Ctrl Pts',(-2.12529269955321,1.89448265541499,9.49394805869999));
#6412=CARTESIAN_POINT('Ctrl Pts',(-1.59897691007952,2.81982132355466,7.38438838139752));
#6413=CARTESIAN_POINT('Ctrl Pts',(-1.07266112060584,4.63767182202801,5.96949854538387));
#6414=CARTESIAN_POINT('Ctrl Pts',(-0.546345331132152,6.90983674793835,5.59034127944055));
#6415=CARTESIAN_POINT('Ctrl Pts',(-0.0200295416584694,9.08860507096528,
6.33831338950149));
#6416=CARTESIAN_POINT('Ctrl Pts',(0.506286247815215,10.6487792451797,8.03311433031102));
#6417=CARTESIAN_POINT('Ctrl Pts',(1.0326020372889,11.2142753892165,10.2662081021742));
#6418=CARTESIAN_POINT('Ctrl Pts',(1.55891782676258,10.6487792451797,12.4993018740374));
#6419=CARTESIAN_POINT('Ctrl Pts',(2.08523361623627,9.0886050709653,14.194102814847));
#6420=CARTESIAN_POINT('Ctrl Pts',(2.61154940570995,6.90983674793834,14.9420749249079));
#6421=CARTESIAN_POINT('Ctrl Pts',(3.13786519518364,4.63767182202801,14.5629176589646));
#6422=CARTESIAN_POINT('Ctrl Pts',(3.66418098465732,2.81982132355465,13.1480278229509));
#6423=CARTESIAN_POINT('Ctrl Pts',(4.19049677413101,1.89448265541498,11.0384681456485));
#6424=CARTESIAN_POINT('Ctrl Pts',(4.71681256360468,2.08471101467815,8.74275325608004));
#6425=CARTESIAN_POINT('Ctrl Pts',(5.24312835307838,3.3446513802314,6.81427096212333));
#6426=CARTESIAN_POINT('Ctrl Pts',(5.76944414255205,5.3705919801484,5.71788673728997));
#6427=CARTESIAN_POINT('Ctrl Pts',(6.29575993202575,7.67417477285421,5.71788673728895));
#6428=CARTESIAN_POINT('Ctrl Pts',(6.82207572149942,9.70011537277266,6.81427096212487));
#6429=CARTESIAN_POINT('Ctrl Pts',(7.34839151097311,10.9600557383222,8.7427532560771));
#6430=CARTESIAN_POINT('Ctrl Pts',(7.8747073004468,11.1502840975933,11.0384681456543));
#6431=CARTESIAN_POINT('Ctrl Pts',(8.40102308992048,10.2249454294372,13.148027822939));
#6432=CARTESIAN_POINT('Ctrl Pts',(8.92733887939416,8.40709493099771,14.562917658989));
#6433=CARTESIAN_POINT('Ctrl Pts',(9.45365466886784,6.13493000501789,14.9420749248578));
#6434=CARTESIAN_POINT('Ctrl Pts',(9.97997045834153,3.9561616821333,14.1941028149495));
#6435=CARTESIAN_POINT('Ctrl Pts',(10.5062862478152,2.39598750762723,12.4993018738273));
#6436=CARTESIAN_POINT('Ctrl Pts',(11.0326020372889,1.83049136418784,10.2662081026046));
#6437=CARTESIAN_POINT('Ctrl Pts',(11.5589178267626,2.39598750700087,8.03311432942944));
#6438=CARTESIAN_POINT('Ctrl Pts',(12.0852336162363,3.95616168372213,6.33831339130741));
#6439=CARTESIAN_POINT('Ctrl Pts',(12.61154940571,6.13493000161398,5.59034127574115));
#6440=CARTESIAN_POINT('Ctrl Pts',(13.1378651951836,8.40709493804338,5.96949855296197));
#6441=CARTESIAN_POINT('Ctrl Pts',(13.6641809846573,10.2249454149688,7.38438836587406));
#6442=CARTESIAN_POINT('Ctrl Pts',(14.190496774131,11.1502841272486,9.49394809049926));
#6443=CARTESIAN_POINT('Ctrl Pts',(14.7168125636047,10.9600556775659,11.7896628831287));
#6444=CARTESIAN_POINT('Ctrl Pts',(15.2431283530784,9.70011549723399,13.7181453756616));
#6445=CARTESIAN_POINT('Ctrl Pts',(15.7694441425521,7.67417451789751,14.8145291937186));
#6446=CARTESIAN_POINT('Ctrl Pts',(16.2957599320257,5.37059250241929,14.8145300269868));
#6447=CARTESIAN_POINT('Ctrl Pts',(16.8220757214994,3.3446503103771,13.7181440952321));
#6448=CARTESIAN_POINT('Ctrl Pts',(17.3483915109731,2.08471320623786,11.7896652978437));
#6449=CARTESIAN_POINT('Ctrl Pts',(17.8747073004468,1.89447816606942,9.49394324567252));
#6450=CARTESIAN_POINT('Ctrl Pts',(18.4010230899205,2.8198305198544,7.38439824076613));
#6451=CARTESIAN_POINT('Ctrl Pts',(18.9273388793942,4.63765298021549,5.96947834756709));
#6452=CARTESIAN_POINT('Ctrl Pts',(19.4536546688679,6.90987534694561,5.59038266649988));
#6453=CARTESIAN_POINT('Ctrl Pts',(19.9799704583415,9.08852492824313,6.33822825438502));
#6454=CARTESIAN_POINT('Ctrl Pts',(20.5062862478152,10.648941808576,8.03329182042749));
#6455=CARTESIAN_POINT('Ctrl Pts',(20.8571634407977,11.0253866956159,9.52159195985228));
#6456=CARTESIAN_POINT('Ctrl Pts',(21.0326020372889,11.0253866956159,10.2662081021742));
#6457=CARTESIAN_POINT('Ctrl Pts',(-18.9696903481015,12.0184298315526,10.2662081021742));
#6458=CARTESIAN_POINT('Ctrl Pts',(-18.7942517516103,12.0184298315526,11.1750396528639));
#6459=CARTESIAN_POINT('Ctrl Pts',(-18.4433745586278,11.5589692572687,12.9915446672008));
#6460=CARTESIAN_POINT('Ctrl Pts',(-17.9170587691541,9.65443410911255,15.0604240895053));
#6461=CARTESIAN_POINT('Ctrl Pts',(-17.3907429796805,6.99532877884549,15.9731892980894));
#6462=CARTESIAN_POINT('Ctrl Pts',(-16.8644271902068,4.22201466394135,15.5104930007101));
#6463=CARTESIAN_POINT('Ctrl Pts',(-16.3381114007331,2.00330916936381,13.7835412891382));
#6464=CARTESIAN_POINT('Ctrl Pts',(-15.8117956112594,0.873889476925023,11.2087800686737));
#6465=CARTESIAN_POINT('Ctrl Pts',(-15.2854798217857,1.1060769339483,8.40678392236536));
#6466=CARTESIAN_POINT('Ctrl Pts',(-14.759164032312,2.64386707202477,6.05301911539166));
#6467=CARTESIAN_POINT('Ctrl Pts',(-14.2328482428383,5.11658887331684,4.71484793596357));
#6468=CARTESIAN_POINT('Ctrl Pts',(-13.7065324533647,7.92817820664652,4.71484896770077));
#6469=CARTESIAN_POINT('Ctrl Pts',(-13.180216663891,10.4008985246382,6.05301752998757));
#6470=CARTESIAN_POINT('Ctrl Pts',(-12.6539008744173,11.9386924253073,8.4067869122208));
#6471=CARTESIAN_POINT('Ctrl Pts',(-12.1275850849436,12.1708718212904,11.2087740698988));
#6472=CARTESIAN_POINT('Ctrl Pts',(-11.6012692954699,11.0414688142261,13.7835535160476));
#6473=CARTESIAN_POINT('Ctrl Pts',(-11.0749535059962,8.82272905166539,15.5104679827411));
#6474=CARTESIAN_POINT('Ctrl Pts',(-10.5486377165226,6.04948518165475,15.9732405475343));
#6475=CARTESIAN_POINT('Ctrl Pts',(-10.0223219270489,3.39023462074606,15.0603186678871));
#6476=CARTESIAN_POINT('Ctrl Pts',(-9.49600613757519,1.48599633137589,12.9917644722719));
#6477=CARTESIAN_POINT('Ctrl Pts',(-8.96969034810151,0.795791722368668,10.2662081016414));
#6478=CARTESIAN_POINT('Ctrl Pts',(-8.44337455862781,1.485996332142,7.54065173342831));
#6479=CARTESIAN_POINT('Ctrl Pts',(-7.91705876915414,3.39023461880273,5.47209753409825));
#6480=CARTESIAN_POINT('Ctrl Pts',(-7.39074297968046,6.04948518581819,4.55917566145673));
#6481=CARTESIAN_POINT('Ctrl Pts',(-6.86442719020676,8.82272904304761,5.02194821219404));
#6482=CARTESIAN_POINT('Ctrl Pts',(-6.33811140073309,11.0414688319228,6.7488627075365));
#6483=CARTESIAN_POINT('Ctrl Pts',(-5.8117956112594,12.170871785018,9.32364209506915));
#6484=CARTESIAN_POINT('Ctrl Pts',(-5.28547982178571,11.9386924996204,12.1256293727861));
#6485=CARTESIAN_POINT('Ctrl Pts',(-4.75916403231203,10.4008983724055,14.4793985091405));
#6486=CARTESIAN_POINT('Ctrl Pts',(-4.23284824283835,7.92817851849246,15.8175675750933));
#6487=CARTESIAN_POINT('Ctrl Pts',(-3.70653245336467,5.11658823451009,15.8175675750921));
#6488=CARTESIAN_POINT('Ctrl Pts',(-3.18021666389098,2.64386838059882,14.4793985091424));
#6489=CARTESIAN_POINT('Ctrl Pts',(-2.6539008744173,1.1060742533794,12.1256293727824));
#6490=CARTESIAN_POINT('Ctrl Pts',(-2.12758508494361,0.873894967991537,9.3236420950764));
#6491=CARTESIAN_POINT('Ctrl Pts',(-1.60126929546993,2.00329792106653,6.74886270752171));
#6492=CARTESIAN_POINT('Ctrl Pts',(-1.07495350599624,4.2220377099832,5.02194821222431));
#6493=CARTESIAN_POINT('Ctrl Pts',(-0.548637716522558,6.99528156712763,4.55917566139474));
#6494=CARTESIAN_POINT('Ctrl Pts',(-0.0223219270488751,9.65453213431721,
5.47209753422524));
#6495=CARTESIAN_POINT('Ctrl Pts',(0.503993862424809,11.5587704206212,7.54065173316817));
#6496=CARTESIAN_POINT('Ctrl Pts',(1.03030965189849,12.2489750311253,10.2662081021742));
#6497=CARTESIAN_POINT('Ctrl Pts',(1.55662544137218,11.5587704206212,12.9917644711803));
#6498=CARTESIAN_POINT('Ctrl Pts',(2.08294123084587,9.65453213431721,15.0603186701232));
#6499=CARTESIAN_POINT('Ctrl Pts',(2.60925702031954,6.99528156712763,15.9732405429537));
#6500=CARTESIAN_POINT('Ctrl Pts',(3.13557280979324,4.22203770998318,15.5104679921241));
#6501=CARTESIAN_POINT('Ctrl Pts',(3.66188859926691,2.00329792106652,13.7835534968268));
#6502=CARTESIAN_POINT('Ctrl Pts',(4.18820438874061,0.873894967991535,11.2087741092721));
#6503=CARTESIAN_POINT('Ctrl Pts',(4.71452017821428,1.1060742533794,8.40678683156602));
#6504=CARTESIAN_POINT('Ctrl Pts',(5.24083596768797,2.64386838059882,6.05301769520609));
#6505=CARTESIAN_POINT('Ctrl Pts',(5.76715175716164,5.11658823451008,4.71484862925638));
#6506=CARTESIAN_POINT('Ctrl Pts',(6.29346754663534,7.92817851849245,4.71484862925513));
#6507=CARTESIAN_POINT('Ctrl Pts',(6.81978333610902,10.4008983724055,6.053017695208));
#6508=CARTESIAN_POINT('Ctrl Pts',(7.3460991255827,11.9386924996204,8.40678683156239));
#6509=CARTESIAN_POINT('Ctrl Pts',(7.87241491505639,12.170871785018,11.2087741092793));
#6510=CARTESIAN_POINT('Ctrl Pts',(8.39873070453007,11.0414688319228,13.783553496812));
#6511=CARTESIAN_POINT('Ctrl Pts',(8.92504649400376,8.82272904304761,15.5104679921544));
#6512=CARTESIAN_POINT('Ctrl Pts',(9.45136228347744,6.04948518581819,15.9732405428917));
#6513=CARTESIAN_POINT('Ctrl Pts',(9.97767807295112,3.39023461880273,15.0603186702502));
#6514=CARTESIAN_POINT('Ctrl Pts',(10.5039938624248,1.48599633214201,12.9917644709202));
#6515=CARTESIAN_POINT('Ctrl Pts',(11.0303096518985,0.795791722368667,10.2662081027071));
#6516=CARTESIAN_POINT('Ctrl Pts',(11.5566254413722,1.48599633137589,7.54065173207658));
#6517=CARTESIAN_POINT('Ctrl Pts',(12.0829412308458,3.39023462074607,5.47209753646132));
#6518=CARTESIAN_POINT('Ctrl Pts',(12.6092570203196,6.04948518165476,4.5591756568142));
#6519=CARTESIAN_POINT('Ctrl Pts',(13.1355728097932,8.82272905166539,5.02194822160738));
#6520=CARTESIAN_POINT('Ctrl Pts',(13.6618885992669,11.0414688142261,6.74886268830085));
#6521=CARTESIAN_POINT('Ctrl Pts',(14.1882043887406,12.1708718212903,9.32364213444966));
#6522=CARTESIAN_POINT('Ctrl Pts',(14.7145201782143,11.9386924253074,12.1256292921277));
#6523=CARTESIAN_POINT('Ctrl Pts',(15.240835967688,10.4008985246382,14.4793986743609));
#6524=CARTESIAN_POINT('Ctrl Pts',(15.7671517571617,7.9281782066465,15.8175672366477));
#6525=CARTESIAN_POINT('Ctrl Pts',(16.2934675466353,5.11658887331682,15.8175682683849));
#6526=CARTESIAN_POINT('Ctrl Pts',(16.819783336109,2.64386707202477,14.4793970889568));
#6527=CARTESIAN_POINT('Ctrl Pts',(17.3460991255827,1.10607693394831,12.1256322819831));
#6528=CARTESIAN_POINT('Ctrl Pts',(17.8724149150564,0.87388947692502,9.32363613567474));
#6529=CARTESIAN_POINT('Ctrl Pts',(18.3987307045301,2.00330916936382,6.74887491521026));
#6530=CARTESIAN_POINT('Ctrl Pts',(18.9250464940037,4.22201466394136,5.02192320363833));
#6531=CARTESIAN_POINT('Ctrl Pts',(19.4513622834774,6.99532877884548,4.5592269062591));
#6532=CARTESIAN_POINT('Ctrl Pts',(19.9776780729511,9.65443410911256,5.47199211484313));
#6533=CARTESIAN_POINT('Ctrl Pts',(20.5039938624248,11.5589692572687,7.54087153714766));
#6534=CARTESIAN_POINT('Ctrl Pts',(20.8548710554073,12.0184298315526,9.35737655148451));
#6535=CARTESIAN_POINT('Ctrl Pts',(21.0303096518985,12.0184298315526,10.2662081021742));
#6536=CARTESIAN_POINT('Ctrl Pts',(-19.7447240968701,12.6400132078441,10.2662081021742));
#6537=CARTESIAN_POINT('Ctrl Pts',(-19.5692855003789,12.6400132078441,11.2775286623238));
#6538=CARTESIAN_POINT('Ctrl Pts',(-19.2184083073964,12.1285212433829,13.2999046745019));
#6539=CARTESIAN_POINT('Ctrl Pts',(-18.6920925179228,10.0086393556897,15.602512565909));
#6540=CARTESIAN_POINT('Ctrl Pts',(-18.1657767284491,7.04880778687935,16.6186123849351));
#6541=CARTESIAN_POINT('Ctrl Pts',(-17.6394609389754,3.96187493613662,16.103536433244));
#6542=CARTESIAN_POINT('Ctrl Pts',(-17.1131451495017,1.4922586425256,14.1813152991222));
#6543=CARTESIAN_POINT('Ctrl Pts',(-16.586829360028,0.235117861288675,11.3153685977046));
#6544=CARTESIAN_POINT('Ctrl Pts',(-16.0605135705543,0.493561867166209,8.19650898389307));
#6545=CARTESIAN_POINT('Ctrl Pts',(-15.5341977810806,2.20525677030406,5.57656046896309));
#6546=CARTESIAN_POINT('Ctrl Pts',(-15.007881991607,4.95761147974642,4.08706080887933));
#6547=CARTESIAN_POINT('Ctrl Pts',(-14.4815662021333,8.08715560221738,4.08706121814656));
#6548=CARTESIAN_POINT('Ctrl Pts',(-13.9552504126596,10.8395088192841,5.57655984006851));
#6549=CARTESIAN_POINT('Ctrl Pts',(-13.4289346231859,12.5512075080354,8.19651016990216));
#6550=CARTESIAN_POINT('Ctrl Pts',(-12.9026188337123,12.8096434035524,11.3153662181278));
#6551=CARTESIAN_POINT('Ctrl Pts',(-12.3763030442385,11.5525194097769,14.1813201492298));
#6552=CARTESIAN_POINT('Ctrl Pts',(-11.8499872547649,9.08286863851945,16.1035265103043));
#6553=CARTESIAN_POINT('Ctrl Pts',(-11.3236714652912,5.99600646245248,16.6186327058768));
#6554=CARTESIAN_POINT('Ctrl Pts',(-10.7973556758175,3.03602877442981,15.6024710771885));
#6555=CARTESIAN_POINT('Ctrl Pts',(-10.2710398863438,0.91644556180598,13.299989934402));
#6556=CARTESIAN_POINT('Ctrl Pts',(-9.74472409687013,0.148187665078963,10.2662081019628));
#6557=CARTESIAN_POINT('Ctrl Pts',(-9.21840830739645,0.91644556257677,7.23242627048267));
#6558=CARTESIAN_POINT('Ctrl Pts',(-8.69209251792277,3.03602877247459,4.92994512622261));
#6559=CARTESIAN_POINT('Ctrl Pts',(-8.16577672844908,5.99600646664137,3.91378350031322));
#6560=CARTESIAN_POINT('Ctrl Pts',(-7.6394609389754,9.08286862984897,4.42888969031004));
#6561=CARTESIAN_POINT('Ctrl Pts',(-7.11314514950171,11.5525194275819,6.35109606274901));
#6562=CARTESIAN_POINT('Ctrl Pts',(-6.58682936002803,12.8096433670582,9.21704997059926));
#6563=CARTESIAN_POINT('Ctrl Pts',(-6.06051357055434,12.5512075828031,12.3359060664417));
#6564=CARTESIAN_POINT('Ctrl Pts',(-5.53419778108066,10.8395086661199,14.9558562987407));
#6565=CARTESIAN_POINT('Ctrl Pts',(-5.00788199160698,8.08715591597131,16.4453551204558));
#6566=CARTESIAN_POINT('Ctrl Pts',(-4.48156620213329,4.95761083703122,16.4453551204553));
#6567=CARTESIAN_POINT('Ctrl Pts',(-3.95525041265961,2.20525808688441,14.9558562987414));
#6568=CARTESIAN_POINT('Ctrl Pts',(-3.42893462318592,0.493559170196666,12.3359060664403));
#6569=CARTESIAN_POINT('Ctrl Pts',(-2.90261883371224,0.235123385951408,9.21704997060214));
#6570=CARTESIAN_POINT('Ctrl Pts',(-2.37630304423856,1.49224732540739,6.35109606274313));
#6571=CARTESIAN_POINT('Ctrl Pts',(-1.84998725476487,3.96189812318202,4.42888969032205));
#6572=CARTESIAN_POINT('Ctrl Pts',(-1.32367146529119,7.04876028630408,3.91378350028863));
#6573=CARTESIAN_POINT('Ctrl Pts',(-0.797355675817504,10.0087379806461,4.92994512627298));
#6574=CARTESIAN_POINT('Ctrl Pts',(-0.27103988634382,12.128321190185,7.23242627037947));
#6575=CARTESIAN_POINT('Ctrl Pts',(0.255275903129863,12.896579088418,10.2662081021742));
#6576=CARTESIAN_POINT('Ctrl Pts',(0.781591692603546,12.128321190185,13.299989933969));
#6577=CARTESIAN_POINT('Ctrl Pts',(1.30790748207723,10.0087379806461,15.6024710780755));
#6578=CARTESIAN_POINT('Ctrl Pts',(1.83422327155091,7.04876028630408,16.6186327040598));
#6579=CARTESIAN_POINT('Ctrl Pts',(2.3605390610246,3.96189812318201,16.1035265140264));
#6580=CARTESIAN_POINT('Ctrl Pts',(2.88685485049829,1.49224732540738,14.1813201416053));
#6581=CARTESIAN_POINT('Ctrl Pts',(3.41317063997197,0.235123385951407,11.3153662337463));
#6582=CARTESIAN_POINT('Ctrl Pts',(3.93948642944565,0.49355917019667,8.1965101379082));
#6583=CARTESIAN_POINT('Ctrl Pts',(4.46580221891934,2.2052580868844,5.57655990560704));
#6584=CARTESIAN_POINT('Ctrl Pts',(4.99211800839302,4.95761083703123,4.08706108389318));
#6585=CARTESIAN_POINT('Ctrl Pts',(5.5184337978667,8.08715591597129,4.08706108389269));
#6586=CARTESIAN_POINT('Ctrl Pts',(6.04474958734038,10.8395086661199,5.57655990560779));
#6587=CARTESIAN_POINT('Ctrl Pts',(6.57106537681407,12.5512075828031,8.19651013790676));
#6588=CARTESIAN_POINT('Ctrl Pts',(7.09738116628776,12.8096433670582,11.3153662337492));
#6589=CARTESIAN_POINT('Ctrl Pts',(7.62369695576144,11.5525194275819,14.1813201415994));
#6590=CARTESIAN_POINT('Ctrl Pts',(8.15001274523513,9.08286862984896,16.1035265140384));
#6591=CARTESIAN_POINT('Ctrl Pts',(8.67632853470882,5.99600646664138,16.6186327040352));
#6592=CARTESIAN_POINT('Ctrl Pts',(9.20264432418249,3.03602877247459,15.6024710781259));
#6593=CARTESIAN_POINT('Ctrl Pts',(9.72896011365618,0.916445562576777,13.2999899338658));
#6594=CARTESIAN_POINT('Ctrl Pts',(10.2552759031299,0.148187665078963,10.2662081023856));
#6595=CARTESIAN_POINT('Ctrl Pts',(10.7815916926035,0.916445561805976,7.23242626994647));
#6596=CARTESIAN_POINT('Ctrl Pts',(11.3079074820772,3.03602877442982,4.92994512715997));
#6597=CARTESIAN_POINT('Ctrl Pts',(11.8342232715509,5.99600646245248,3.91378349847164));
#6598=CARTESIAN_POINT('Ctrl Pts',(12.3605390610246,9.08286863851947,4.4288896940441));
#6599=CARTESIAN_POINT('Ctrl Pts',(12.8868548504983,11.5525194097769,6.35109605511865));
#6600=CARTESIAN_POINT('Ctrl Pts',(13.413170639972,12.8096434035524,9.21704998622064));
#6601=CARTESIAN_POINT('Ctrl Pts',(13.9394864294457,12.5512075080354,12.3359060344463));
#6602=CARTESIAN_POINT('Ctrl Pts',(14.4658022189193,10.8395088192841,14.9558563642799));
#6603=CARTESIAN_POINT('Ctrl Pts',(14.992118008393,8.08715560221737,16.4453549862019));
#6604=CARTESIAN_POINT('Ctrl Pts',(15.5184337978667,4.9576114797464,16.4453553954691));
#6605=CARTESIAN_POINT('Ctrl Pts',(16.0447495873404,2.20525677030405,14.9558557353854));
#6606=CARTESIAN_POINT('Ctrl Pts',(16.5710653768141,0.493561867166209,12.3359072204554));
#6607=CARTESIAN_POINT('Ctrl Pts',(17.0973811662878,0.235117861288674,9.21704760664382));
#6608=CARTESIAN_POINT('Ctrl Pts',(17.6236969557614,1.4922586425256,6.35110090522623));
#6609=CARTESIAN_POINT('Ctrl Pts',(18.1500127452351,3.96187493613663,4.42887977110448));
#6610=CARTESIAN_POINT('Ctrl Pts',(18.6763285347088,7.04880778687935,3.91380381941334));
#6611=CARTESIAN_POINT('Ctrl Pts',(19.2026443241825,10.0086393556897,4.92990363843943));
#6612=CARTESIAN_POINT('Ctrl Pts',(19.7289601136562,12.1285212433829,7.23251152984658));
#6613=CARTESIAN_POINT('Ctrl Pts',(20.0798373066386,12.6400132078441,9.25488754202469));
#6614=CARTESIAN_POINT('Ctrl Pts',(20.2552759031298,12.6400132078441,10.2662081021742));
#6615=CARTESIAN_POINT('Ctrl Pts',(-20.7138122396522,12.4160945610234,10.2662081021742));
#6616=CARTESIAN_POINT('Ctrl Pts',(-20.538373643161,12.4160945610234,11.2408846067237));
#6617=CARTESIAN_POINT('Ctrl Pts',(-20.1874964501786,11.9234097510006,13.1886963350883));
#6618=CARTESIAN_POINT('Ctrl Pts',(-19.6611806607048,9.8810581004343,15.4073432872781));
#6619=CARTESIAN_POINT('Ctrl Pts',(-19.1348648712312,7.02955135660707,16.3861208997243));
#6620=CARTESIAN_POINT('Ctrl Pts',(-18.6085490817575,4.05556523698548,15.8899610759315));
#6621=CARTESIAN_POINT('Ctrl Pts',(-18.0822332922838,1.67632104728412,14.0380438270458));
#6622=CARTESIAN_POINT('Ctrl Pts',(-17.5559175028101,0.465178955365346,11.2769833767237));
#6623=CARTESIAN_POINT('Ctrl Pts',(-17.0296017133364,0.714167149390354,8.27224020810767));
#6624=CARTESIAN_POINT('Ctrl Pts',(-16.5032859238627,2.36322766355062,5.74816399917117));
#6625=CARTESIAN_POINT('Ctrl Pts',(-15.976970134389,5.01486925380052,4.31316578561841));
#6626=CARTESIAN_POINT('Ctrl Pts',(-15.4506543449154,8.02989786004729,4.31316710813318));
#6627=CARTESIAN_POINT('Ctrl Pts',(-14.9243385554417,10.6815378132754,5.74816196694792));
#6628=CARTESIAN_POINT('Ctrl Pts',(-14.398022765968,12.3306024799635,8.272244040603));
#6629=CARTESIAN_POINT('Ctrl Pts',(-13.8717069764943,12.5795817775447,11.276975687295));
#6630=CARTESIAN_POINT('Ctrl Pts',(-13.3453911870206,11.3684581001844,14.0380594999119));
#6631=CARTESIAN_POINT('Ctrl Pts',(-12.8190753975469,8.98917609114738,15.8899290067425));
#6632=CARTESIAN_POINT('Ctrl Pts',(-12.2927596080733,6.01526749622851,16.3861865954599));
#6633=CARTESIAN_POINT('Ctrl Pts',(-11.7664438185996,3.1636004708241,15.4072080579704));
#6634=CARTESIAN_POINT('Ctrl Pts',(-11.2401280291259,1.12157644391819,13.1889786533539));
#6635=CARTESIAN_POINT('Ctrl Pts',(-10.7138122396522,0.381430421865054,10.2662081014912));
#6636=CARTESIAN_POINT('Ctrl Pts',(-10.1874964501785,1.1215764447637,7.34343755272727));
#6637=CARTESIAN_POINT('Ctrl Pts',(-9.66118066070484,3.16360046867936,5.12520814334897));
#6638=CARTESIAN_POINT('Ctrl Pts',(-9.13486487123116,6.01526750082342,4.14622961483952));
#6639=CARTESIAN_POINT('Ctrl Pts',(-8.60854908175746,8.98917608163649,4.6424871855396));
#6640=CARTESIAN_POINT('Ctrl Pts',(-8.08223329228379,11.3684581197151,6.49435672909347));
#6641=CARTESIAN_POINT('Ctrl Pts',(-7.55591750281009,12.5795817375133,9.25544046657416));
#6642=CARTESIAN_POINT('Ctrl Pts',(-7.02960171333642,12.330602561978,12.2601722671361));
#6643=CARTESIAN_POINT('Ctrl Pts',(-6.50328592386273,10.6815376452661,14.7842540256155));
#6644=CARTESIAN_POINT('Ctrl Pts',(-5.97697013438905,8.02989820421129,16.2192495300461));
#6645=CARTESIAN_POINT('Ctrl Pts',(-5.45065434491537,5.01486854879121,16.2192495300445));
#6646=CARTESIAN_POINT('Ctrl Pts',(-4.92433855544167,2.36322910773836,14.784254025618));
#6647=CARTESIAN_POINT('Ctrl Pts',(-4.39802276596799,0.714164191021466,12.2601722671314));
#6648=CARTESIAN_POINT('Ctrl Pts',(-3.87170697649431,0.465185015496949,9.25544046658345));
#6649=CARTESIAN_POINT('Ctrl Pts',(-3.34539118702063,1.6763086332728,6.49435672907451));
#6650=CARTESIAN_POINT('Ctrl Pts',(-2.81907539754694,4.0555906713972,4.6424871855784));
#6651=CARTESIAN_POINT('Ctrl Pts',(-2.29275960807326,7.02949925211648,4.14622961476005));
#6652=CARTESIAN_POINT('Ctrl Pts',(-1.76644381859957,9.88116628445271,5.12520814351175));
#6653=CARTESIAN_POINT('Ctrl Pts',(-1.24012802912589,11.9231903079747,7.34343755239381));
#6654=CARTESIAN_POINT('Ctrl Pts',(-0.713812239652205,12.6633363316798,10.2662081021742));
#6655=CARTESIAN_POINT('Ctrl Pts',(-0.187496450178523,11.9231903079747,13.1889786519547));
#6656=CARTESIAN_POINT('Ctrl Pts',(0.338819339295166,9.88116628445271,15.4072080608367));
#6657=CARTESIAN_POINT('Ctrl Pts',(0.865135128768847,7.02949925211648,16.3861865895884));
#6658=CARTESIAN_POINT('Ctrl Pts',(1.39145091824253,4.0555906713972,15.8899290187701));
#6659=CARTESIAN_POINT('Ctrl Pts',(1.91776670771622,1.67630863327279,14.0380594752739));
#6660=CARTESIAN_POINT('Ctrl Pts',(2.4440824971899,0.465185015496951,11.276975737765));
#6661=CARTESIAN_POINT('Ctrl Pts',(2.97039828666358,0.714164191021463,8.27224393721703));
#6662=CARTESIAN_POINT('Ctrl Pts',(3.49671407613727,2.36322910773836,5.74816217873048));
#6663=CARTESIAN_POINT('Ctrl Pts',(4.02302986561095,5.0148685487912,4.31316667430399));
#6664=CARTESIAN_POINT('Ctrl Pts',(4.54934565508464,8.02989820421128,4.3131666743024));
#6665=CARTESIAN_POINT('Ctrl Pts',(5.07566144455832,10.6815376452661,5.74816217873292));
#6666=CARTESIAN_POINT('Ctrl Pts',(5.60197723403201,12.330602561978,8.27224393721239));
#6667=CARTESIAN_POINT('Ctrl Pts',(6.12829302350569,12.5795817375133,11.2769757377743));
#6668=CARTESIAN_POINT('Ctrl Pts',(6.65460881297937,11.3684581197151,14.038059475255));
#6669=CARTESIAN_POINT('Ctrl Pts',(7.18092460245306,8.98917608163649,15.8899290188089));
#6670=CARTESIAN_POINT('Ctrl Pts',(7.70724039192674,6.01526750082342,16.3861865895089));
#6671=CARTESIAN_POINT('Ctrl Pts',(8.23355618140043,3.16360046867936,15.4072080609995));
#6672=CARTESIAN_POINT('Ctrl Pts',(8.75987197087411,1.1215764447637,13.1889786516212));
#6673=CARTESIAN_POINT('Ctrl Pts',(9.28618776034779,0.381430421865052,10.2662081028573));
#6674=CARTESIAN_POINT('Ctrl Pts',(9.81250354982149,1.12157644391819,7.34343755099458));
#6675=CARTESIAN_POINT('Ctrl Pts',(10.3388193392952,3.16360047082409,5.12520814637803));
#6676=CARTESIAN_POINT('Ctrl Pts',(10.8651351287689,6.01526749622852,4.14622960888857));
#6677=CARTESIAN_POINT('Ctrl Pts',(11.3914509182425,8.98917609114738,4.64248719760592));
#6678=CARTESIAN_POINT('Ctrl Pts',(11.9177667077162,11.3684581001844,6.49435670443657));
#6679=CARTESIAN_POINT('Ctrl Pts',(12.4440824971899,12.5795817775447,9.25544051705342));
#6680=CARTESIAN_POINT('Ctrl Pts',(12.9703982866636,12.3306024799635,12.2601721637455));
#6681=CARTESIAN_POINT('Ctrl Pts',(13.4967140761373,10.6815378132754,14.7842542374005));
#6682=CARTESIAN_POINT('Ctrl Pts',(14.023029865611,8.02989786004727,16.2192490962153));
#6683=CARTESIAN_POINT('Ctrl Pts',(14.5493456550846,5.0148692538005,16.21925041873));
#6684=CARTESIAN_POINT('Ctrl Pts',(15.0756614445583,2.36322766355062,14.7842522051773));
#6685=CARTESIAN_POINT('Ctrl Pts',(15.601977234032,0.714167149390356,12.2601759962408));
#6686=CARTESIAN_POINT('Ctrl Pts',(16.1282930235057,0.46517895536534,9.25543282762478));
#6687=CARTESIAN_POINT('Ctrl Pts',(16.6546088129794,1.67632104728413,6.49437237730269));
#6688=CARTESIAN_POINT('Ctrl Pts',(17.1809246024531,4.05556523698548,4.64245512841697));
#6689=CARTESIAN_POINT('Ctrl Pts',(17.7072403919268,7.02955135660707,4.14629530462416));
#6690=CARTESIAN_POINT('Ctrl Pts',(18.2335561814004,9.8810581004343,5.12507291707035));
#6691=CARTESIAN_POINT('Ctrl Pts',(18.7598719708741,11.9234097510006,7.34371986926018));
#6692=CARTESIAN_POINT('Ctrl Pts',(19.1107491638566,12.4160945610234,9.29153159762474));
#6693=CARTESIAN_POINT('Ctrl Pts',(19.2861877603478,12.4160945610234,10.2662081021742));
#6694=CARTESIAN_POINT('Ctrl Pts',(-21.,11.8215826768434,10.2662081021742));
#6695=CARTESIAN_POINT('Ctrl Pts',(-20.8245614035088,11.8215826768434,11.1423372082236));
#6696=CARTESIAN_POINT('Ctrl Pts',(-20.4736842105263,11.3785434349997,12.8940021805135));
#6697=CARTESIAN_POINT('Ctrl Pts',(-19.9473684210526,9.54224664734747,14.8886522715445));
#6698=CARTESIAN_POINT('Ctrl Pts',(-19.421052631579,6.9783848758886,15.7687789642738));
#6699=CARTESIAN_POINT('Ctrl Pts',(-18.8947368421052,4.30441716130508,15.322628929525));
#6700=CARTESIAN_POINT('Ctrl Pts',(-18.3684210526316,2.16518578050098,13.6575517805422));
#6701=CARTESIAN_POINT('Ctrl Pts',(-17.8421052631579,1.07622381336149,11.1750141268389));
#6702=CARTESIAN_POINT('Ctrl Pts',(-17.3157894736842,1.30009366399148,8.47339120268354));
#6703=CARTESIAN_POINT('Ctrl Pts',(-16.7894736842105,2.78279902034384,6.20393874295387));
#6704=CARTESIAN_POINT('Ctrl Pts',(-16.2631578947368,5.16694563809232,4.91370280999657));
#6705=CARTESIAN_POINT('Ctrl Pts',(-15.7368421052632,7.87782141228263,4.91370342697971));
#6706=CARTESIAN_POINT('Ctrl Pts',(-15.2105263157895,10.2619666809626,6.20393779487563));
#6707=CARTESIAN_POINT('Ctrl Pts',(-14.6842105263158,11.7446754594104,8.47339299062945));
#6708=CARTESIAN_POINT('Ctrl Pts',(-14.1578947368421,11.9685379784868,11.1750105395485));
#6709=CARTESIAN_POINT('Ctrl Pts',(-13.6315789473684,10.8795911867729,13.6575590922666));
#6710=CARTESIAN_POINT('Ctrl Pts',(-13.1052631578947,8.74032863907908,15.3226139692546));
#6711=CARTESIAN_POINT('Ctrl Pts',(-12.5789473684211,6.06642481255227,15.7688096072721));
#6712=CARTESIAN_POINT('Ctrl Pts',(-12.0526315789474,3.50243095315069,14.8885893974933));
#6713=CARTESIAN_POINT('Ctrl Pts',(-11.5263157894737,1.66640415994231,12.8941326374224));
#6714=CARTESIAN_POINT('Ctrl Pts',(-11.,1.0009232890457,10.2662081018556));
#6715=CARTESIAN_POINT('Ctrl Pts',(-10.4736842105263,1.66640416063908,7.63828356773443));
#6716=CARTESIAN_POINT('Ctrl Pts',(-9.94736842105264,3.50243095138322,5.64382680544198));
#6717=CARTESIAN_POINT('Ctrl Pts',(-9.42105263157895,6.06642481633893,4.7636065998526));
#6718=CARTESIAN_POINT('Ctrl Pts',(-8.89473684210527,8.74032863124119,5.20980222946469));
#6719=CARTESIAN_POINT('Ctrl Pts',(-8.36842105263158,10.8795912028682,6.87485712358485));
#6720=CARTESIAN_POINT('Ctrl Pts',(-7.84210526315789,11.968537945497,9.35740564125021));
#6721=CARTESIAN_POINT('Ctrl Pts',(-7.31578947368422,11.7446755269984,12.0590232619531));
#6722=CARTESIAN_POINT('Ctrl Pts',(-6.78947368421053,10.2619665425062,14.3284783106703));
#6723=CARTESIAN_POINT('Ctrl Pts',(-6.26315789473684,7.87782169590793,15.6187129797607));
#6724=CARTESIAN_POINT('Ctrl Pts',(-5.73684210526316,5.16694505709463,15.6187129797599));
#6725=CARTESIAN_POINT('Ctrl Pts',(-5.21052631578947,2.782800210498,14.3284783106715));
#6726=CARTESIAN_POINT('Ctrl Pts',(-4.68421052631579,1.30009122600162,12.0590232619509));
#6727=CARTESIAN_POINT('Ctrl Pts',(-4.15789473684211,1.07622880751197,9.35740564125455));
#6728=CARTESIAN_POINT('Ctrl Pts',(-3.63157894736843,2.16517555012239,6.87485712357599));
#6729=CARTESIAN_POINT('Ctrl Pts',(-3.10526315789474,4.30443812178711,5.20980222948279));
#6730=CARTESIAN_POINT('Ctrl Pts',(-2.57894736842106,6.97834193661205,4.76360659981552));
#6731=CARTESIAN_POINT('Ctrl Pts',(-2.05263157894737,9.54233580172614,5.64382680551793));
#6732=CARTESIAN_POINT('Ctrl Pts',(-1.52631578947369,11.3783625921458,7.63828356757886));
#6733=CARTESIAN_POINT('Ctrl Pts',(-1.,12.0438434644038,10.2662081021742));
#6734=CARTESIAN_POINT('Ctrl Pts',(-0.47368421052632,11.3783625921459,12.8941326367696));
#6735=CARTESIAN_POINT('Ctrl Pts',(0.0526315789473631,9.54233580172614,14.8885893988306));
#6736=CARTESIAN_POINT('Ctrl Pts',(0.578947368421052,6.97834193661205,15.7688096045329));
#6737=CARTESIAN_POINT('Ctrl Pts',(1.10526315789473,4.3044381217871,15.3226139748657));
#6738=CARTESIAN_POINT('Ctrl Pts',(1.63157894736842,2.16517555012238,13.6575590807725));
#6739=CARTESIAN_POINT('Ctrl Pts',(2.1578947368421,1.07622880751197,11.1750105630939));
#6740=CARTESIAN_POINT('Ctrl Pts',(2.68421052631579,1.30009122600162,8.47339294239756));
#6741=CARTESIAN_POINT('Ctrl Pts',(3.21052631578947,2.782800210498,6.203937893677));
#6742=CARTESIAN_POINT('Ctrl Pts',(3.73684210526315,5.16694505709462,4.91370322458856));
#6743=CARTESIAN_POINT('Ctrl Pts',(4.26315789473684,7.87782169590794,4.91370322458781));
#6744=CARTESIAN_POINT('Ctrl Pts',(4.78947368421052,10.2619665425062,6.20393789367814));
#6745=CARTESIAN_POINT('Ctrl Pts',(5.31578947368421,11.7446755269984,8.47339294239539));
#6746=CARTESIAN_POINT('Ctrl Pts',(5.84210526315788,11.968537945497,11.1750105630982));
#6747=CARTESIAN_POINT('Ctrl Pts',(6.36842105263158,10.8795912028682,13.6575590807636));
#6748=CARTESIAN_POINT('Ctrl Pts',(6.89473684210526,8.74032863124118,15.3226139748838));
#6749=CARTESIAN_POINT('Ctrl Pts',(7.42105263157895,6.06642481633893,15.7688096044959));
#6750=CARTESIAN_POINT('Ctrl Pts',(7.94736842105263,3.50243095138322,14.8885893989065));
#6751=CARTESIAN_POINT('Ctrl Pts',(8.47368421052631,1.66640416063909,12.894132636614));
#6752=CARTESIAN_POINT('Ctrl Pts',(9.,1.0009232890457,10.2662081024929));
#6753=CARTESIAN_POINT('Ctrl Pts',(9.52631578947368,1.66640415994231,7.63828356692609));
#6754=CARTESIAN_POINT('Ctrl Pts',(10.0526315789474,3.50243095315069,5.64382680685511));
#6755=CARTESIAN_POINT('Ctrl Pts',(10.578947368421,6.06642481255228,4.76360659707634));
#6756=CARTESIAN_POINT('Ctrl Pts',(11.1052631578947,8.74032863907909,5.20980223509391));
#6757=CARTESIAN_POINT('Ctrl Pts',(11.6315789473684,10.8795911867729,6.87485711208184));
#6758=CARTESIAN_POINT('Ctrl Pts',(12.1578947368421,11.9685379784868,9.35740566479993));
#6759=CARTESIAN_POINT('Ctrl Pts',(12.6842105263158,11.7446754594104,12.059023213719));
#6760=CARTESIAN_POINT('Ctrl Pts',(13.2105263157895,10.2619666809626,14.3284784094728));
#6761=CARTESIAN_POINT('Ctrl Pts',(13.7368421052632,7.8778214122826,15.6187127773688));
#6762=CARTESIAN_POINT('Ctrl Pts',(14.2631578947369,5.16694563809232,15.6187133943519));
#6763=CARTESIAN_POINT('Ctrl Pts',(14.7894736842105,2.78279902034383,14.3284774613946));
#6764=CARTESIAN_POINT('Ctrl Pts',(15.3157894736842,1.30009366399149,12.0590250016649));
#6765=CARTESIAN_POINT('Ctrl Pts',(15.8421052631579,1.07622381336148,9.3574020775096));
#6766=CARTESIAN_POINT('Ctrl Pts',(16.3684210526316,2.16518578050099,6.87486442380621));
#6767=CARTESIAN_POINT('Ctrl Pts',(16.8947368421052,4.30441716130507,5.2097872748235));
#6768=CARTESIAN_POINT('Ctrl Pts',(17.421052631579,6.9783848758886,4.76363724007471));
#6769=CARTESIAN_POINT('Ctrl Pts',(17.9473684210526,9.54224664734746,5.64376393280394));
#6770=CARTESIAN_POINT('Ctrl Pts',(18.4736842105263,11.3785434349997,7.63841402383501));
#6771=CARTESIAN_POINT('Ctrl Pts',(18.8245614035088,11.8215826768433,9.39007899612484));
#6772=CARTESIAN_POINT('Ctrl Pts',(19.,11.8215826768434,10.2662081021742));
#6773=CARTESIAN_POINT('Ctrl Pts',(-21.,11.5223833765015,10.2662081021742));
#6774=CARTESIAN_POINT('Ctrl Pts',(-20.8245614035088,11.5223833765015,11.0929430110137));
#6775=CARTESIAN_POINT('Ctrl Pts',(-20.4736842105263,11.1043754458166,12.7456006386873));
#6776=CARTESIAN_POINT('Ctrl Pts',(-19.9473684210526,9.37174604195822,14.627693070812));
#6777=CARTESIAN_POINT('Ctrl Pts',(-19.421052631579,6.95264079877442,15.4581010648004));
#6778=CARTESIAN_POINT('Ctrl Pts',(-18.8947368421052,4.4296403847971,15.0371536204255));
#6779=CARTESIAN_POINT('Ctrl Pts',(-18.3684210526316,2.41118846113653,13.4660782459265));
#6780=CARTESIAN_POINT('Ctrl Pts',(-17.8421052631579,1.38370759752575,11.1237050325294));
#6781=CARTESIAN_POINT('Ctrl Pts',(-17.3157894736842,1.59493822839275,8.57461107686665));
#6782=CARTESIAN_POINT('Ctrl Pts',(-16.7894736842105,2.9939316339387,6.43329006745293));
#6783=CARTESIAN_POINT('Ctrl Pts',(-16.2631578947368,5.2434721166514,5.21589900368628));
#6784=CARTESIAN_POINT('Ctrl Pts',(-15.7368421052632,7.80129492555693,5.21589976806491));
#6785=CARTESIAN_POINT('Ctrl Pts',(-15.2105263157895,10.0508340962501,6.43328889288153));
#6786=CARTESIAN_POINT('Ctrl Pts',(-14.6842105263158,11.4498308299117,8.57461329194773));
#6787=CARTESIAN_POINT('Ctrl Pts',(-14.1578947368421,11.6610543305691,11.1237005882441));
#6788=CARTESIAN_POINT('Ctrl Pts',(-13.6315789473684,10.6335882256263,13.4660873044149));
#6789=CARTESIAN_POINT('Ctrl Pts',(-13.1052631578947,8.61510599100168,15.0371350857393));
#6790=CARTESIAN_POINT('Ctrl Pts',(-12.5789473684211,6.09216771054517,15.4581390317312));
#6791=CARTESIAN_POINT('Ctrl Pts',(-12.0526315789474,3.67293400690476,14.6276150452767));
#6792=CARTESIAN_POINT('Ctrl Pts',(-11.5263157894737,1.94056718272496,12.7457630293102));
#6793=CARTESIAN_POINT('Ctrl Pts',(-11.,1.31265859936127,10.2662081017794));
#6794=CARTESIAN_POINT('Ctrl Pts',(-10.4736842105263,1.9405671834026,7.78665317603972));
#6795=CARTESIAN_POINT('Ctrl Pts',(-9.94736842105264,3.67293400518582,5.90480115732107));
#6796=CARTESIAN_POINT('Ctrl Pts',(-9.42105263157895,6.09216771422783,5.07427717605678));
#6797=CARTESIAN_POINT('Ctrl Pts',(-8.89473684210527,8.61510598337903,5.49528111163513));
#6798=CARTESIAN_POINT('Ctrl Pts',(-8.36842105263158,10.6335882412796,7.06632891418456));
#6799=CARTESIAN_POINT('Ctrl Pts',(-7.84210526315789,11.6610542984852,9.40871558692863));
#6800=CARTESIAN_POINT('Ctrl Pts',(-7.31578947368422,11.4498308956436,11.9578029721578));
#6801=CARTESIAN_POINT('Ctrl Pts',(-6.78947368421053,10.0508339615961,14.0991271890608));
#6802=CARTESIAN_POINT('Ctrl Pts',(-6.26315789473684,7.80129520139315,15.3165166870263));
#6803=CARTESIAN_POINT('Ctrl Pts',(-5.73684210526316,5.24347155160944,15.3165166870254));
#6804=CARTESIAN_POINT('Ctrl Pts',(-5.21052631578947,2.99393279140807,14.0991271890622));
#6805=CARTESIAN_POINT('Ctrl Pts',(-4.68421052631579,1.59493585735657,11.9578029721551));
#6806=CARTESIAN_POINT('Ctrl Pts',(-4.15789473684211,1.38371245452358,9.408715586934));
#6807=CARTESIAN_POINT('Ctrl Pts',(-3.63157894736843,2.41117851171133,7.0663289141736));
#6808=CARTESIAN_POINT('Ctrl Pts',(-3.10526315789474,4.42966076964857,5.49528111165755));
#6809=CARTESIAN_POINT('Ctrl Pts',(-2.57894736842106,6.95259903872457,5.07427717601085));
#6810=CARTESIAN_POINT('Ctrl Pts',(-2.05263157894737,9.3718327479206,5.90480115741515));
#6811=CARTESIAN_POINT('Ctrl Pts',(-1.52631578947369,11.1041995693883,7.78665317584699));
#6812=CARTESIAN_POINT('Ctrl Pts',(-1.,11.732108154076,10.2662081021742));
#6813=CARTESIAN_POINT('Ctrl Pts',(-0.47368421052632,11.1041995693883,12.7457630285015));
#6814=CARTESIAN_POINT('Ctrl Pts',(0.052631578947363,9.37183274792061,14.6276150469333));
#6815=CARTESIAN_POINT('Ctrl Pts',(0.578947368421052,6.95259903872456,15.4581390283376));
#6816=CARTESIAN_POINT('Ctrl Pts',(1.10526315789473,4.42966076964857,15.0371350926909));
#6817=CARTESIAN_POINT('Ctrl Pts',(1.63157894736842,2.41117851171132,13.4660872901749));
#6818=CARTESIAN_POINT('Ctrl Pts',(2.1578947368421,1.38371245452358,11.1237006174145));
#6819=CARTESIAN_POINT('Ctrl Pts',(2.68421052631579,1.59493585735657,8.57461323219337));
#6820=CARTESIAN_POINT('Ctrl Pts',(3.21052631578947,2.99393279140808,6.43328901528626));
#6821=CARTESIAN_POINT('Ctrl Pts',(3.73684210526315,5.24347155160942,5.21589951732309));
#6822=CARTESIAN_POINT('Ctrl Pts',(4.26315789473684,7.80129520139315,5.21589951732216));
#6823=CARTESIAN_POINT('Ctrl Pts',(4.78947368421052,10.0508339615961,6.43328901528768));
#6824=CARTESIAN_POINT('Ctrl Pts',(5.31578947368421,11.4498308956436,8.57461323219068));
#6825=CARTESIAN_POINT('Ctrl Pts',(5.84210526315788,11.6610542984852,11.1237006174198));
#6826=CARTESIAN_POINT('Ctrl Pts',(6.36842105263158,10.6335882412796,13.4660872901639));
#6827=CARTESIAN_POINT('Ctrl Pts',(6.89473684210526,8.61510598337902,15.0371350927133));
#6828=CARTESIAN_POINT('Ctrl Pts',(7.42105263157895,6.09216771422785,15.4581390282917));
#6829=CARTESIAN_POINT('Ctrl Pts',(7.94736842105263,3.67293400518582,14.6276150470274));
#6830=CARTESIAN_POINT('Ctrl Pts',(8.47368421052631,1.94056718340261,12.7457630283087));
#6831=CARTESIAN_POINT('Ctrl Pts',(9.,1.31265859936126,10.266208102569));
#6832=CARTESIAN_POINT('Ctrl Pts',(9.52631578947368,1.94056718272496,7.78665317503828));
#6833=CARTESIAN_POINT('Ctrl Pts',(10.0526315789474,3.67293400690476,5.90480115907178));
#6834=CARTESIAN_POINT('Ctrl Pts',(10.578947368421,6.09216771054518,5.07427717261729));
#6835=CARTESIAN_POINT('Ctrl Pts',(11.1052631578947,8.61510599100168,5.49528111860915));
#6836=CARTESIAN_POINT('Ctrl Pts',(11.6315789473684,10.6335882256264,7.06632889993352));
#6837=CARTESIAN_POINT('Ctrl Pts',(12.1578947368421,11.6610543305691,9.40871561610432));
#6838=CARTESIAN_POINT('Ctrl Pts',(12.6842105263158,11.4498308299117,11.9578029124007));
#6839=CARTESIAN_POINT('Ctrl Pts',(13.2105263157895,10.0508340962501,14.0991273114669));
#6840=CARTESIAN_POINT('Ctrl Pts',(13.7368421052632,7.80129492555691,15.3165164362836));
#6841=CARTESIAN_POINT('Ctrl Pts',(14.2631578947369,5.24347211665139,15.3165172006622));
#6842=CARTESIAN_POINT('Ctrl Pts',(14.7894736842105,2.9939316339387,14.0991261368955));
#6843=CARTESIAN_POINT('Ctrl Pts',(15.3157894736842,1.59493822839275,11.9578051274818));
#6844=CARTESIAN_POINT('Ctrl Pts',(15.8421052631579,1.38370759752574,9.4087111718191));
#6845=CARTESIAN_POINT('Ctrl Pts',(16.3684210526316,2.41118846113653,7.06633795842197));
#6846=CARTESIAN_POINT('Ctrl Pts',(16.8947368421052,4.42964038479711,5.49526258392294));
#6847=CARTESIAN_POINT('Ctrl Pts',(17.421052631579,6.95264079877441,5.07431513954803));
#6848=CARTESIAN_POINT('Ctrl Pts',(17.9473684210526,9.37174604195823,5.90472313353644));
#6849=CARTESIAN_POINT('Ctrl Pts',(18.4736842105263,11.1043754458165,7.78681556566119));
#6850=CARTESIAN_POINT('Ctrl Pts',(18.8245614035088,11.5223833765015,9.43947319333481));
#6851=CARTESIAN_POINT('Ctrl Pts',(19.,11.5223833765015,10.2662081021742));
#6852=CARTESIAN_POINT('',(-21.,11.5223833765015,10.2662081021742));
#6853=CARTESIAN_POINT('Origin',(-20.,11.5223833765015,10.2662081021742));
#6854=CARTESIAN_POINT('',(19.,11.5223833765015,10.2662081021742));
#6855=CARTESIAN_POINT('Ctrl Pts',(-21.,11.5223833765015,10.2662081021742));
#6856=CARTESIAN_POINT('Ctrl Pts',(-20.8245614035088,11.5223833765015,11.0929430110137));
#6857=CARTESIAN_POINT('Ctrl Pts',(-20.4736842105263,11.1043754458166,12.7456006386873));
#6858=CARTESIAN_POINT('Ctrl Pts',(-19.9473684210526,9.37174604195822,14.627693070812));
#6859=CARTESIAN_POINT('Ctrl Pts',(-19.421052631579,6.95264079877442,15.4581010648004));
#6860=CARTESIAN_POINT('Ctrl Pts',(-18.8947368421052,4.4296403847971,15.0371536204255));
#6861=CARTESIAN_POINT('Ctrl Pts',(-18.3684210526316,2.41118846113653,13.4660782459265));
#6862=CARTESIAN_POINT('Ctrl Pts',(-17.8421052631579,1.38370759752575,11.1237050325294));
#6863=CARTESIAN_POINT('Ctrl Pts',(-17.3157894736842,1.59493822839275,8.57461107686665));
#6864=CARTESIAN_POINT('Ctrl Pts',(-16.7894736842105,2.9939316339387,6.43329006745293));
#6865=CARTESIAN_POINT('Ctrl Pts',(-16.2631578947368,5.2434721166514,5.21589900368628));
#6866=CARTESIAN_POINT('Ctrl Pts',(-15.7368421052632,7.80129492555693,5.21589976806491));
#6867=CARTESIAN_POINT('Ctrl Pts',(-15.2105263157895,10.0508340962501,6.43328889288153));
#6868=CARTESIAN_POINT('Ctrl Pts',(-14.6842105263158,11.4498308299117,8.57461329194773));
#6869=CARTESIAN_POINT('Ctrl Pts',(-14.1578947368421,11.6610543305691,11.1237005882441));
#6870=CARTESIAN_POINT('Ctrl Pts',(-13.6315789473684,10.6335882256263,13.4660873044149));
#6871=CARTESIAN_POINT('Ctrl Pts',(-13.1052631578947,8.61510599100168,15.0371350857393));
#6872=CARTESIAN_POINT('Ctrl Pts',(-12.5789473684211,6.09216771054517,15.4581390317312));
#6873=CARTESIAN_POINT('Ctrl Pts',(-12.0526315789474,3.67293400690476,14.6276150452767));
#6874=CARTESIAN_POINT('Ctrl Pts',(-11.5263157894737,1.94056718272496,12.7457630293102));
#6875=CARTESIAN_POINT('Ctrl Pts',(-11.,1.31265859936127,10.2662081017794));
#6876=CARTESIAN_POINT('Ctrl Pts',(-10.4736842105263,1.9405671834026,7.78665317603972));
#6877=CARTESIAN_POINT('Ctrl Pts',(-9.94736842105264,3.67293400518582,5.90480115732107));
#6878=CARTESIAN_POINT('Ctrl Pts',(-9.42105263157895,6.09216771422783,5.07427717605678));
#6879=CARTESIAN_POINT('Ctrl Pts',(-8.89473684210527,8.61510598337903,5.49528111163513));
#6880=CARTESIAN_POINT('Ctrl Pts',(-8.36842105263158,10.6335882412796,7.06632891418456));
#6881=CARTESIAN_POINT('Ctrl Pts',(-7.84210526315789,11.6610542984852,9.40871558692863));
#6882=CARTESIAN_POINT('Ctrl Pts',(-7.31578947368422,11.4498308956436,11.9578029721578));
#6883=CARTESIAN_POINT('Ctrl Pts',(-6.78947368421053,10.0508339615961,14.0991271890608));
#6884=CARTESIAN_POINT('Ctrl Pts',(-6.26315789473684,7.80129520139315,15.3165166870263));
#6885=CARTESIAN_POINT('Ctrl Pts',(-5.73684210526316,5.24347155160944,15.3165166870254));
#6886=CARTESIAN_POINT('Ctrl Pts',(-5.21052631578947,2.99393279140807,14.0991271890622));
#6887=CARTESIAN_POINT('Ctrl Pts',(-4.68421052631579,1.59493585735657,11.9578029721551));
#6888=CARTESIAN_POINT('Ctrl Pts',(-4.15789473684211,1.38371245452358,9.408715586934));
#6889=CARTESIAN_POINT('Ctrl Pts',(-3.63157894736843,2.41117851171133,7.0663289141736));
#6890=CARTESIAN_POINT('Ctrl Pts',(-3.10526315789474,4.42966076964857,5.49528111165755));
#6891=CARTESIAN_POINT('Ctrl Pts',(-2.57894736842106,6.95259903872457,5.07427717601085));
#6892=CARTESIAN_POINT('Ctrl Pts',(-2.05263157894737,9.3718327479206,5.90480115741515));
#6893=CARTESIAN_POINT('Ctrl Pts',(-1.52631578947369,11.1041995693883,7.78665317584699));
#6894=CARTESIAN_POINT('Ctrl Pts',(-1.,11.732108154076,10.2662081021742));
#6895=CARTESIAN_POINT('Ctrl Pts',(-0.47368421052632,11.1041995693883,12.7457630285015));
#6896=CARTESIAN_POINT('Ctrl Pts',(0.052631578947363,9.37183274792061,14.6276150469333));
#6897=CARTESIAN_POINT('Ctrl Pts',(0.578947368421052,6.95259903872456,15.4581390283376));
#6898=CARTESIAN_POINT('Ctrl Pts',(1.10526315789473,4.42966076964857,15.0371350926909));
#6899=CARTESIAN_POINT('Ctrl Pts',(1.63157894736842,2.41117851171132,13.4660872901749));
#6900=CARTESIAN_POINT('Ctrl Pts',(2.1578947368421,1.38371245452358,11.1237006174145));
#6901=CARTESIAN_POINT('Ctrl Pts',(2.68421052631579,1.59493585735657,8.57461323219337));
#6902=CARTESIAN_POINT('Ctrl Pts',(3.21052631578947,2.99393279140808,6.43328901528626));
#6903=CARTESIAN_POINT('Ctrl Pts',(3.73684210526315,5.24347155160942,5.21589951732309));
#6904=CARTESIAN_POINT('Ctrl Pts',(4.26315789473684,7.80129520139315,5.21589951732216));
#6905=CARTESIAN_POINT('Ctrl Pts',(4.78947368421052,10.0508339615961,6.43328901528768));
#6906=CARTESIAN_POINT('Ctrl Pts',(5.31578947368421,11.4498308956436,8.57461323219068));
#6907=CARTESIAN_POINT('Ctrl Pts',(5.84210526315788,11.6610542984852,11.1237006174198));
#6908=CARTESIAN_POINT('Ctrl Pts',(6.36842105263158,10.6335882412796,13.4660872901639));
#6909=CARTESIAN_POINT('Ctrl Pts',(6.89473684210526,8.61510598337902,15.0371350927133));
#6910=CARTESIAN_POINT('Ctrl Pts',(7.42105263157895,6.09216771422785,15.4581390282917));
#6911=CARTESIAN_POINT('Ctrl Pts',(7.94736842105263,3.67293400518582,14.6276150470274));
#6912=CARTESIAN_POINT('Ctrl Pts',(8.47368421052631,1.94056718340261,12.7457630283087));
#6913=CARTESIAN_POINT('Ctrl Pts',(9.,1.31265859936126,10.266208102569));
#6914=CARTESIAN_POINT('Ctrl Pts',(9.52631578947368,1.94056718272496,7.78665317503828));
#6915=CARTESIAN_POINT('Ctrl Pts',(10.0526315789474,3.67293400690476,5.90480115907178));
#6916=CARTESIAN_POINT('Ctrl Pts',(10.578947368421,6.09216771054518,5.07427717261729));
#6917=CARTESIAN_POINT('Ctrl Pts',(11.1052631578947,8.61510599100168,5.49528111860915));
#6918=CARTESIAN_POINT('Ctrl Pts',(11.6315789473684,10.6335882256264,7.06632889993352));
#6919=CARTESIAN_POINT('Ctrl Pts',(12.1578947368421,11.6610543305691,9.40871561610432));
#6920=CARTESIAN_POINT('Ctrl Pts',(12.6842105263158,11.4498308299117,11.9578029124007));
#6921=CARTESIAN_POINT('Ctrl Pts',(13.2105263157895,10.0508340962501,14.0991273114669));
#6922=CARTESIAN_POINT('Ctrl Pts',(13.7368421052632,7.80129492555691,15.3165164362836));
#6923=CARTESIAN_POINT('Ctrl Pts',(14.2631578947369,5.24347211665139,15.3165172006622));
#6924=CARTESIAN_POINT('Ctrl Pts',(14.7894736842105,2.9939316339387,14.0991261368955));
#6925=CARTESIAN_POINT('Ctrl Pts',(15.3157894736842,1.59493822839275,11.9578051274818));
#6926=CARTESIAN_POINT('Ctrl Pts',(15.8421052631579,1.38370759752574,9.4087111718191));
#6927=CARTESIAN_POINT('Ctrl Pts',(16.3684210526316,2.41118846113653,7.06633795842197));
#6928=CARTESIAN_POINT('Ctrl Pts',(16.8947368421052,4.42964038479711,5.49526258392294));
#6929=CARTESIAN_POINT('Ctrl Pts',(17.421052631579,6.95264079877441,5.07431513954803));
#6930=CARTESIAN_POINT('Ctrl Pts',(17.9473684210526,9.37174604195823,5.90472313353644));
#6931=CARTESIAN_POINT('Ctrl Pts',(18.4736842105263,11.1043754458165,7.78681556566119));
#6932=CARTESIAN_POINT('Ctrl Pts',(18.8245614035088,11.5223833765015,9.43947319333481));
#6933=CARTESIAN_POINT('Ctrl Pts',(19.,11.5223833765015,10.2662081021742));
#6934=CARTESIAN_POINT('Origin',(20.,11.5223833765015,10.2662081021742));
#6935=CARTESIAN_POINT('Origin',(20.,11.5223833765015,10.2662081021742));
#6936=CARTESIAN_POINT('Origin',(-20.,11.5223833765015,10.2662081021742));
#6937=CARTESIAN_POINT('',(0.,0.,0.));
#6938=CARTESIAN_POINT('Origin',(-24.3,-11.4095206243716,16.));
#6939=CARTESIAN_POINT('',(-24.3,-11.4095206243716,16.));
#6940=CARTESIAN_POINT('',(24.3,-11.4095206243716,16.));
#6941=CARTESIAN_POINT('',(-12.15,-11.4095206243716,16.));
#6942=CARTESIAN_POINT('',(-24.3,-11.4095206243716,15.9));
#6943=CARTESIAN_POINT('',(-24.3,-11.4095206243716,16.));
#6944=CARTESIAN_POINT('',(24.3,-11.4095206243716,15.9));
#6945=CARTESIAN_POINT('',(-24.3,-11.4095206243716,15.9));
#6946=CARTESIAN_POINT('',(24.3,-11.4095206243716,16.));
#6947=CARTESIAN_POINT('Origin',(-24.3,-2.80952062437159,16.));
#6948=CARTESIAN_POINT('',(-24.3,-2.80952062437159,16.));
#6949=CARTESIAN_POINT('',(-24.3,-4.95952062437158,16.));
#6950=CARTESIAN_POINT('',(-24.3,-2.80952062437159,15.9));
#6951=CARTESIAN_POINT('',(-24.3,-2.80952062437159,16.));
#6952=CARTESIAN_POINT('',(-24.3,-2.80952062437159,15.9));
#6953=CARTESIAN_POINT('Origin',(24.3,-2.80952062437159,16.));
#6954=CARTESIAN_POINT('',(24.3,-2.80952062437159,16.));
#6955=CARTESIAN_POINT('',(12.15,-2.80952062437159,16.));
#6956=CARTESIAN_POINT('',(24.3,-2.80952062437159,15.9));
#6957=CARTESIAN_POINT('',(24.3,-2.80952062437159,16.));
#6958=CARTESIAN_POINT('',(24.3,-2.80952062437159,15.9));
#6959=CARTESIAN_POINT('Origin',(24.3,-11.4095206243716,16.));
#6960=CARTESIAN_POINT('',(24.3,-9.2595206243716,16.));
#6961=CARTESIAN_POINT('',(24.3,-11.4095206243716,15.9));
#6962=CARTESIAN_POINT('Origin',(0.,-7.10952062437159,15.9));
#6963=CARTESIAN_POINT('',(-25.,-2.10952062437159,15.9));
#6964=CARTESIAN_POINT('',(25.,-2.10952062437159,15.9));
#6965=CARTESIAN_POINT('',(-12.5,-2.10952062437159,15.9));
#6966=CARTESIAN_POINT('',(-25.,-12.1095206243716,15.9));
#6967=CARTESIAN_POINT('',(-25.,-9.60952062437159,15.9));
#6968=CARTESIAN_POINT('',(25.,-12.1095206243716,15.9));
#6969=CARTESIAN_POINT('',(12.5,-12.1095206243716,15.9));
#6970=CARTESIAN_POINT('',(25.,-4.60952062437159,15.9));
#6971=CARTESIAN_POINT('Origin',(-25.,-12.1095206243716,16.));
#6972=CARTESIAN_POINT('',(-25.,-2.10952062437159,15.));
#6973=CARTESIAN_POINT('',(-25.,-2.10952062437159,16.));
#6974=CARTESIAN_POINT('',(-25.,-12.1095206243716,15.));
#6975=CARTESIAN_POINT('',(-25.,-2.10952062437159,15.));
#6976=CARTESIAN_POINT('',(-25.,-12.1095206243716,16.));
#6977=CARTESIAN_POINT('Origin',(-25.,-2.10952062437159,16.));
#6978=CARTESIAN_POINT('',(25.,-2.10952062437159,15.));
#6979=CARTESIAN_POINT('',(25.,-2.10952062437159,16.));
#6980=CARTESIAN_POINT('',(25.,-2.10952062437159,15.));
#6981=CARTESIAN_POINT('Origin',(22.,-5.60952062437159,16.));
#6982=CARTESIAN_POINT('',(22.,-5.60952062437159,16.));
#6983=CARTESIAN_POINT('',(22.,-8.60952062437159,16.));
#6984=CARTESIAN_POINT('',(22.,-6.35952062437159,16.));
#6985=CARTESIAN_POINT('',(22.,-5.60952062437159,15.9));
#6986=CARTESIAN_POINT('',(22.,-5.60952062437159,16.));
#6987=CARTESIAN_POINT('',(22.,-8.60952062437159,15.9));
#6988=CARTESIAN_POINT('',(22.,-5.60952062437159,15.9));
#6989=CARTESIAN_POINT('',(22.,-8.60952062437159,16.));
#6990=CARTESIAN_POINT('Origin',(-22.,-5.60952062437159,16.));
#6991=CARTESIAN_POINT('',(-22.,-5.60952062437159,16.));
#6992=CARTESIAN_POINT('',(-11.,-5.60952062437159,16.));
#6993=CARTESIAN_POINT('',(-22.,-5.60952062437159,15.9));
#6994=CARTESIAN_POINT('',(-22.,-5.60952062437159,16.));
#6995=CARTESIAN_POINT('',(-22.,-5.60952062437159,15.9));
#6996=CARTESIAN_POINT('Origin',(-22.,-8.60952062437159,16.));
#6997=CARTESIAN_POINT('',(-22.,-8.60952062437159,16.));
#6998=CARTESIAN_POINT('',(-22.,-7.85952062437159,16.));
#6999=CARTESIAN_POINT('',(-22.,-8.60952062437159,15.9));
#7000=CARTESIAN_POINT('',(-22.,-8.60952062437159,16.));
#7001=CARTESIAN_POINT('',(-22.,-8.60952062437159,15.9));
#7002=CARTESIAN_POINT('Origin',(22.,-8.60952062437159,16.));
#7003=CARTESIAN_POINT('',(11.,-8.60952062437159,16.));
#7004=CARTESIAN_POINT('',(22.,-8.60952062437159,15.9));
#7005=CARTESIAN_POINT('Origin',(0.,-7.10952062437159,15.9));
#7006=CARTESIAN_POINT('Origin',(25.,-12.1095206243716,16.));
#7007=CARTESIAN_POINT('',(25.,-12.1095206243716,15.));
#7008=CARTESIAN_POINT('',(-25.,-12.1095206243716,15.));
#7009=CARTESIAN_POINT('',(25.,-12.1095206243716,16.));
#7010=CARTESIAN_POINT('Origin',(25.,-2.10952062437159,16.));
#7011=CARTESIAN_POINT('',(25.,-12.1095206243716,15.));
#7012=CARTESIAN_POINT('Origin',(0.,-7.10952062437159,16.));
#7013=CARTESIAN_POINT('Origin',(0.,-7.10952062437159,15.));
#7014=CARTESIAN_POINT('',(42.,22.,16.));
#7015=CARTESIAN_POINT('',(42.,-22.,16.));
#7016=CARTESIAN_POINT('',(-42.,22.,16.));
#7017=CARTESIAN_POINT('',(-42.,-22.,16.));
#7018=CARTESIAN_POINT('',(0.,0.,0.));
#7019=CARTESIAN_POINT('',(0.,0.,0.));
#7020=CARTESIAN_POINT('',(0.,0.,0.));
#7021=CARTESIAN_POINT('',(0.,0.,0.));
#7022=CARTESIAN_POINT('',(0.,0.,0.));
#7023=CARTESIAN_POINT('',(0.,0.,0.));
#7024=UNCERTAINTY_MEASURE_WITH_UNIT(LENGTH_MEASURE(0.01),#7048,
'DISTANCE_ACCURACY_VALUE',
'Maximum model space distance between geometric entities at asserted c
onnectivities');
#7025=UNCERTAINTY_MEASURE_WITH_UNIT(LENGTH_MEASURE(0.01),#7048,
'DISTANCE_ACCURACY_VALUE',
'Maximum model space distance between geometric entities at asserted c
onnectivities');
#7026=UNCERTAINTY_MEASURE_WITH_UNIT(LENGTH_MEASURE(0.01),#7048,
'DISTANCE_ACCURACY_VALUE',
'Maximum model space distance between geometric entities at asserted c
onnectivities');
#7027=UNCERTAINTY_MEASURE_WITH_UNIT(LENGTH_MEASURE(0.01),#7048,
'DISTANCE_ACCURACY_VALUE',
'Maximum model space distance between geometric entities at asserted c
onnectivities');
#7028=UNCERTAINTY_MEASURE_WITH_UNIT(LENGTH_MEASURE(0.01),#7048,
'DISTANCE_ACCURACY_VALUE',
'Maximum model space distance between geometric entities at asserted c
onnectivities');
#7029=UNCERTAINTY_MEASURE_WITH_UNIT(LENGTH_MEASURE(0.01),#7048,
'DISTANCE_ACCURACY_VALUE',
'Maximum model space distance between geometric entities at asserted c
onnectivities');
#7030=UNCERTAINTY_MEASURE_WITH_UNIT(LENGTH_MEASURE(0.01),#7048,
'DISTANCE_ACCURACY_VALUE',
'Maximum model space distance between geometric entities at asserted c
onnectivities');
#7031=UNCERTAINTY_MEASURE_WITH_UNIT(LENGTH_MEASURE(0.01),#7048,
'DISTANCE_ACCURACY_VALUE',
'Maximum model space distance between geometric entities at asserted c
onnectivities');
#7032=UNCERTAINTY_MEASURE_WITH_UNIT(LENGTH_MEASURE(0.01),#7048,
'DISTANCE_ACCURACY_VALUE',
'Maximum model space distance between geometric entities at asserted c
onnectivities');
#7033=UNCERTAINTY_MEASURE_WITH_UNIT(LENGTH_MEASURE(0.01),#7048,
'DISTANCE_ACCURACY_VALUE',
'Maximum model space distance between geometric entities at asserted c
onnectivities');
#7034=UNCERTAINTY_MEASURE_WITH_UNIT(LENGTH_MEASURE(0.01),#7048,
'DISTANCE_ACCURACY_VALUE',
'Maximum model space distance between geometric entities at asserted c
onnectivities');
#7035=UNCERTAINTY_MEASURE_WITH_UNIT(LENGTH_MEASURE(0.01),#7048,
'DISTANCE_ACCURACY_VALUE',
'Maximum model space distance between geometric entities at asserted c
onnectivities');
#7036=(
GEOMETRIC_REPRESENTATION_CONTEXT(3)
GLOBAL_UNCERTAINTY_ASSIGNED_CONTEXT((#7024))
GLOBAL_UNIT_ASSIGNED_CONTEXT((#7048,#7050,#7051))
REPRESENTATION_CONTEXT('','3D')
);
#7037=(
GEOMETRIC_REPRESENTATION_CONTEXT(3)
GLOBAL_UNCERTAINTY_ASSIGNED_CONTEXT((#7025))
GLOBAL_UNIT_ASSIGNED_CONTEXT((#7048,#7050,#7051))
REPRESENTATION_CONTEXT('','3D')
);
#7038=(
GEOMETRIC_REPRESENTATION_CONTEXT(3)
GLOBAL_UNCERTAINTY_ASSIGNED_CONTEXT((#7026))
GLOBAL_UNIT_ASSIGNED_CONTEXT((#7048,#7050,#7051))
REPRESENTATION_CONTEXT('','3D')
);
#7039=(
GEOMETRIC_REPRESENTATION_CONTEXT(3)
GLOBAL_UNCERTAINTY_ASSIGNED_CONTEXT((#7027))
GLOBAL_UNIT_ASSIGNED_CONTEXT((#7048,#7050,#7051))
REPRESENTATION_CONTEXT('','3D')
);
#7040=(
GEOMETRIC_REPRESENTATION_CONTEXT(3)
GLOBAL_UNCERTAINTY_ASSIGNED_CONTEXT((#7028))
GLOBAL_UNIT_ASSIGNED_CONTEXT((#7048,#7050,#7051))
REPRESENTATION_CONTEXT('','3D')
);
#7041=(
GEOMETRIC_REPRESENTATION_CONTEXT(3)
GLOBAL_UNCERTAINTY_ASSIGNED_CONTEXT((#7029))
GLOBAL_UNIT_ASSIGNED_CONTEXT((#7048,#7050,#7051))
REPRESENTATION_CONTEXT('','3D')
);
#7042=(
GEOMETRIC_REPRESENTATION_CONTEXT(3)
GLOBAL_UNCERTAINTY_ASSIGNED_CONTEXT((#7030))
GLOBAL_UNIT_ASSIGNED_CONTEXT((#7048,#7050,#7051))
REPRESENTATION_CONTEXT('','3D')
);
#7043=(
GEOMETRIC_REPRESENTATION_CONTEXT(3)
GLOBAL_UNCERTAINTY_ASSIGNED_CONTEXT((#7031))
GLOBAL_UNIT_ASSIGNED_CONTEXT((#7048,#7050,#7051))
REPRESENTATION_CONTEXT('','3D')
);
#7044=(
GEOMETRIC_REPRESENTATION_CONTEXT(3)
GLOBAL_UNCERTAINTY_ASSIGNED_CONTEXT((#7032))
GLOBAL_UNIT_ASSIGNED_CONTEXT((#7048,#7050,#7051))
REPRESENTATION_CONTEXT('','3D')
);
#7045=(
GEOMETRIC_REPRESENTATION_CONTEXT(3)
GLOBAL_UNCERTAINTY_ASSIGNED_CONTEXT((#7033))
GLOBAL_UNIT_ASSIGNED_CONTEXT((#7048,#7050,#7051))
REPRESENTATION_CONTEXT('','3D')
);
#7046=(
GEOMETRIC_REPRESENTATION_CONTEXT(3)
GLOBAL_UNCERTAINTY_ASSIGNED_CONTEXT((#7034))
GLOBAL_UNIT_ASSIGNED_CONTEXT((#7048,#7050,#7051))
REPRESENTATION_CONTEXT('','3D')
);
#7047=(
GEOMETRIC_REPRESENTATION_CONTEXT(3)
GLOBAL_UNCERTAINTY_ASSIGNED_CONTEXT((#7035))
GLOBAL_UNIT_ASSIGNED_CONTEXT((#7048,#7050,#7051))
REPRESENTATION_CONTEXT('','3D')
);
#7048=(
LENGTH_UNIT()
NAMED_UNIT(*)
SI_UNIT(.MILLI.,.METRE.)
);
#7049=(
LENGTH_UNIT()
NAMED_UNIT(*)
SI_UNIT($,.METRE.)
);
#7050=(
NAMED_UNIT(*)
PLANE_ANGLE_UNIT()
SI_UNIT($,.RADIAN.)
);
#7051=(
NAMED_UNIT(*)
SI_UNIT($,.STERADIAN.)
SOLID_ANGLE_UNIT()
);
#7052=SHAPE_DEFINITION_REPRESENTATION(#7063,#7084);
#7053=SHAPE_DEFINITION_REPRESENTATION(#7064,#7085);
#7054=SHAPE_DEFINITION_REPRESENTATION(#7065,#7086);
#7055=SHAPE_DEFINITION_REPRESENTATION(#7066,#7087);
#7056=SHAPE_DEFINITION_REPRESENTATION(#7067,#7088);
#7057=SHAPE_DEFINITION_REPRESENTATION(#7068,#7089);
#7058=SHAPE_DEFINITION_REPRESENTATION(#7069,#7090);
#7059=SHAPE_DEFINITION_REPRESENTATION(#7070,#7091);
#7060=SHAPE_DEFINITION_REPRESENTATION(#7071,#7092);
#7061=SHAPE_DEFINITION_REPRESENTATION(#7072,#7093);
#7062=SHAPE_DEFINITION_REPRESENTATION(#7073,#7094);
#7063=PRODUCT_DEFINITION_SHAPE('',$,#7096);
#7064=PRODUCT_DEFINITION_SHAPE('',$,#7097);
#7065=PRODUCT_DEFINITION_SHAPE('',$,#7098);
#7066=PRODUCT_DEFINITION_SHAPE('',$,#7099);
#7067=PRODUCT_DEFINITION_SHAPE('',$,#7100);
#7068=PRODUCT_DEFINITION_SHAPE('',$,#7101);
#7069=PRODUCT_DEFINITION_SHAPE('',$,#7102);
#7070=PRODUCT_DEFINITION_SHAPE('',$,#7103);
#7071=PRODUCT_DEFINITION_SHAPE('',$,#7104);
#7072=PRODUCT_DEFINITION_SHAPE('',$,#7105);
#7073=PRODUCT_DEFINITION_SHAPE('',$,#7106);
#7074=PRODUCT_DEFINITION_SHAPE($,$,#41);
#7075=PRODUCT_DEFINITION_SHAPE($,$,#42);
#7076=PRODUCT_DEFINITION_SHAPE($,$,#43);
#7077=PRODUCT_DEFINITION_SHAPE($,$,#44);
#7078=PRODUCT_DEFINITION_SHAPE($,$,#45);
#7079=PRODUCT_DEFINITION_SHAPE($,$,#46);
#7080=PRODUCT_DEFINITION_SHAPE($,$,#47);
#7081=PRODUCT_DEFINITION_SHAPE($,$,#48);
#7082=PRODUCT_DEFINITION_SHAPE($,$,#49);
#7083=PRODUCT_DEFINITION_SHAPE($,$,#50);
#7084=SHAPE_REPRESENTATION('',(#3518,#3882,#3883,#3884,#3885,#3886,#3887,
#3888,#3889,#3890,#3891),#7036);
#7085=SHAPE_REPRESENTATION('',(#3519),#7037);
#7086=SHAPE_REPRESENTATION('',(#3580),#7038);
#7087=SHAPE_REPRESENTATION('',(#3641),#7039);
#7088=SHAPE_REPRESENTATION('',(#3702),#7040);
#7089=SHAPE_REPRESENTATION('',(#3763),#7041);
#7090=SHAPE_REPRESENTATION('',(#3780),#7042);
#7091=SHAPE_REPRESENTATION('',(#3810),#7043);
#7092=SHAPE_REPRESENTATION('',(#3827),#7044);
#7093=SHAPE_REPRESENTATION('',(#3860),#7045);
#7094=SHAPE_REPRESENTATION('',(#3865),#7046);
#7095=PRODUCT_DEFINITION_CONTEXT('part definition',#7130,'design');
#7096=PRODUCT_DEFINITION('MAS-278','MAS-278',#7107,#7095);
#7097=PRODUCT_DEFINITION('BHS JIS B 1111 - M5x14 Steel 4.6 Plain',
'M5x14 Steel 4.6 Plain v1',#7108,#7095);
#7098=PRODUCT_DEFINITION('BHS JIS B 1111 - M5x14 Steel 4.6 Plain_1',
'M5x14 Steel 4.6 Plain v1 (1)',#7109,#7095);
#7099=PRODUCT_DEFINITION('BHS JIS B 1111 - M5x14 Steel 4.6 Plain_2',
'M5x14 Steel 4.6 Plain v1 (2)',#7110,#7095);
#7100=PRODUCT_DEFINITION('BHS JIS B 1111 - M5x14 Steel 4.6 Plain_3',
'M5x14 Steel 4.6 Plain v1 (3)',#7111,#7095);
#7101=PRODUCT_DEFINITION('Front_Block','Front_Block',#7112,#7095);
#7102=PRODUCT_DEFINITION('Left_Block','Left_Block',#7113,#7095);
#7103=PRODUCT_DEFINITION('End_Block','End_Block',#7114,#7095);
#7104=PRODUCT_DEFINITION('Right_Block','Right_Block',#7115,#7095);
#7105=PRODUCT_DEFINITION('Spring','Spring',#7116,#7095);
#7106=PRODUCT_DEFINITION('Circuit','Circuit',#7117,#7095);
#7107=PRODUCT_DEFINITION_FORMATION('',$,#7132);
#7108=PRODUCT_DEFINITION_FORMATION('',$,#7133);
#7109=PRODUCT_DEFINITION_FORMATION('',$,#7134);
#7110=PRODUCT_DEFINITION_FORMATION('',$,#7135);
#7111=PRODUCT_DEFINITION_FORMATION('',$,#7136);
#7112=PRODUCT_DEFINITION_FORMATION('',$,#7137);
#7113=PRODUCT_DEFINITION_FORMATION('',$,#7138);
#7114=PRODUCT_DEFINITION_FORMATION('',$,#7139);
#7115=PRODUCT_DEFINITION_FORMATION('',$,#7140);
#7116=PRODUCT_DEFINITION_FORMATION('',$,#7141);
#7117=PRODUCT_DEFINITION_FORMATION('',$,#7142);
#7118=PRODUCT_RELATED_PRODUCT_CATEGORY('MAS-278','MAS-278',(#7132));
#7119=PRODUCT_RELATED_PRODUCT_CATEGORY('M5x14 Steel 4.6 Plain v1',
'M5x14 Steel 4.6 Plain v1',(#7133));
#7120=PRODUCT_RELATED_PRODUCT_CATEGORY('M5x14 Steel 4.6 Plain v1 (1)',
'M5x14 Steel 4.6 Plain v1 (1)',(#7134));
#7121=PRODUCT_RELATED_PRODUCT_CATEGORY('M5x14 Steel 4.6 Plain v1 (2)',
'M5x14 Steel 4.6 Plain v1 (2)',(#7135));
#7122=PRODUCT_RELATED_PRODUCT_CATEGORY('M5x14 Steel 4.6 Plain v1 (3)',
'M5x14 Steel 4.6 Plain v1 (3)',(#7136));
#7123=PRODUCT_RELATED_PRODUCT_CATEGORY('Front_Block','Front_Block',(#7137));
#7124=PRODUCT_RELATED_PRODUCT_CATEGORY('Left_Block','Left_Block',(#7138));
#7125=PRODUCT_RELATED_PRODUCT_CATEGORY('End_Block','End_Block',(#7139));
#7126=PRODUCT_RELATED_PRODUCT_CATEGORY('Right_Block','Right_Block',(#7140));
#7127=PRODUCT_RELATED_PRODUCT_CATEGORY('Spring','Spring',(#7141));
#7128=PRODUCT_RELATED_PRODUCT_CATEGORY('Circuit','Circuit',(#7142));
#7129=APPLICATION_PROTOCOL_DEFINITION('international standard',
'automotive_design',2009,#7130);
#7130=APPLICATION_CONTEXT(
'Core Data for Automotive Mechanical Design Process');
#7131=PRODUCT_CONTEXT('part definition',#7130,'mechanical');
#7132=PRODUCT('MAS-278','MAS-278',$,(#7131));
#7133=PRODUCT('BHS JIS B 1111 - M5x14 Steel 4.6 Plain',
'M5x14 Steel 4.6 Plain v1','Binding Head Screw JIS B 1111 - M5x14',(#7131));
#7134=PRODUCT('BHS JIS B 1111 - M5x14 Steel 4.6 Plain_1',
'M5x14 Steel 4.6 Plain v1 (1)','Binding Head Screw JIS B 1111 - M5x14',
(#7131));
#7135=PRODUCT('BHS JIS B 1111 - M5x14 Steel 4.6 Plain_2',
'M5x14 Steel 4.6 Plain v1 (2)','Binding Head Screw JIS B 1111 - M5x14',
(#7131));
#7136=PRODUCT('BHS JIS B 1111 - M5x14 Steel 4.6 Plain_3',
'M5x14 Steel 4.6 Plain v1 (3)','Binding Head Screw JIS B 1111 - M5x14',
(#7131));
#7137=PRODUCT('Front_Block','Front_Block',$,(#7131));
#7138=PRODUCT('Left_Block','Left_Block',$,(#7131));
#7139=PRODUCT('End_Block','End_Block',$,(#7131));
#7140=PRODUCT('Right_Block','Right_Block',$,(#7131));
#7141=PRODUCT('Spring','Spring',$,(#7131));
#7142=PRODUCT('Circuit','Circuit',$,(#7131));
#7143=PRESENTATION_STYLE_ASSIGNMENT((#7147));
#7144=PRESENTATION_STYLE_ASSIGNMENT((#7148));
#7145=PRESENTATION_STYLE_ASSIGNMENT((#7149));
#7146=PRESENTATION_STYLE_ASSIGNMENT((#7150));
#7147=SURFACE_STYLE_USAGE(.BOTH.,#7151);
#7148=SURFACE_STYLE_USAGE(.BOTH.,#7152);
#7149=SURFACE_STYLE_USAGE(.BOTH.,#7153);
#7150=SURFACE_STYLE_USAGE(.BOTH.,#7154);
#7151=SURFACE_SIDE_STYLE('',(#7155));
#7152=SURFACE_SIDE_STYLE('',(#7156));
#7153=SURFACE_SIDE_STYLE('',(#7157));
#7154=SURFACE_SIDE_STYLE('',(#7158));
#7155=SURFACE_STYLE_FILL_AREA(#7159);
#7156=SURFACE_STYLE_FILL_AREA(#7160);
#7157=SURFACE_STYLE_FILL_AREA(#7161);
#7158=SURFACE_STYLE_FILL_AREA(#7162);
#7159=FILL_AREA_STYLE('Steel - Satin',(#7163));
#7160=FILL_AREA_STYLE('Steel - Satin (2)',(#7164));
#7161=FILL_AREA_STYLE('Steel - Satin (1) (1)',(#7165));
#7162=FILL_AREA_STYLE('Steel - Satin (1)',(#7166));
#7163=FILL_AREA_STYLE_COLOUR('Steel - Satin',#7167);
#7164=FILL_AREA_STYLE_COLOUR('Steel - Satin (2)',#7168);
#7165=FILL_AREA_STYLE_COLOUR('Steel - Satin (1) (1)',#7169);
#7166=FILL_AREA_STYLE_COLOUR('Steel - Satin (1)',#7170);
#7167=COLOUR_RGB('Steel - Satin',0.627450980392157,0.627450980392157,0.627450980392157);
#7168=COLOUR_RGB('Steel - Satin (2)',0.776470588235294,0.63921568627451,
0.63921568627451);
#7169=COLOUR_RGB('Steel - Satin (1) (1)',0.290196078431373,0.290196078431373,
0.290196078431373);
#7170=COLOUR_RGB('Steel - Satin (1)',0.803921568627451,0.803921568627451,
0.803921568627451);
#7171=COLOUR_RGB('Dark Blue',0.08,0.2,0.34);
#7172=FILL_AREA_STYLE_COLOUR('',#7171);
#7173=FILL_AREA_STYLE('',(#7172));
#7174=SURFACE_STYLE_FILL_AREA(#7173);
#7175=SURFACE_SIDE_STYLE('',(#7174));
#7176=SURFACE_STYLE_USAGE(.BOTH.,#7175);
#7177=PRESENTATION_STYLE_ASSIGNMENT((#7176));
#7178=COLOUR_RGB('Light Blue',0.38,0.62,0.78);
#7179=FILL_AREA_STYLE_COLOUR('',#7178);
#7180=FILL_AREA_STYLE('',(#7179));
#7181=SURFACE_STYLE_FILL_AREA(#7180);
#7182=SURFACE_SIDE_STYLE('',(#7181));
#7183=SURFACE_STYLE_USAGE(.BOTH.,#7182);
#7184=PRESENTATION_STYLE_ASSIGNMENT((#7183));
#7185=COLOUR_RGB('Sky Blue',0.24,0.69,0.87);
#7186=FILL_AREA_STYLE_COLOUR('',#7185);
#7187=FILL_AREA_STYLE('',(#7186));
#7188=SURFACE_STYLE_FILL_AREA(#7187);
#7189=SURFACE_SIDE_STYLE('',(#7188));
#7190=SURFACE_STYLE_USAGE(.BOTH.,#7189);
#7191=PRESENTATION_STYLE_ASSIGNMENT((#7190));
#7192=COLOUR_RGB('Grey',0.48,0.52,0.57);
#7193=FILL_AREA_STYLE_COLOUR('',#7192);
#7194=FILL_AREA_STYLE('',(#7193));
#7195=SURFACE_STYLE_FILL_AREA(#7194);
#7196=SURFACE_SIDE_STYLE('',(#7195));
#7197=SURFACE_STYLE_USAGE(.BOTH.,#7196);
#7198=PRESENTATION_STYLE_ASSIGNMENT((#7197));
#7199=COLOUR_RGB('Black',0.12,0.14,0.17);
#7200=FILL_AREA_STYLE_COLOUR('',#7199);
#7201=FILL_AREA_STYLE('',(#7200));
#7202=SURFACE_STYLE_FILL_AREA(#7201);
#7203=SURFACE_SIDE_STYLE('',(#7202));
#7204=SURFACE_STYLE_USAGE(.BOTH.,#7203);
#7205=PRESENTATION_STYLE_ASSIGNMENT((#7204));
#7206=COLOUR_RGB('Off White',0.89,0.88,0.83);
#7207=FILL_AREA_STYLE_COLOUR('',#7206);
#7208=FILL_AREA_STYLE('',(#7207));
#7209=SURFACE_STYLE_FILL_AREA(#7208);
#7210=SURFACE_SIDE_STYLE('',(#7209));
#7211=SURFACE_STYLE_USAGE(.BOTH.,#7210);
#7212=PRESENTATION_STYLE_ASSIGNMENT((#7211));
ENDSEC;
END-ISO-10303-21;
